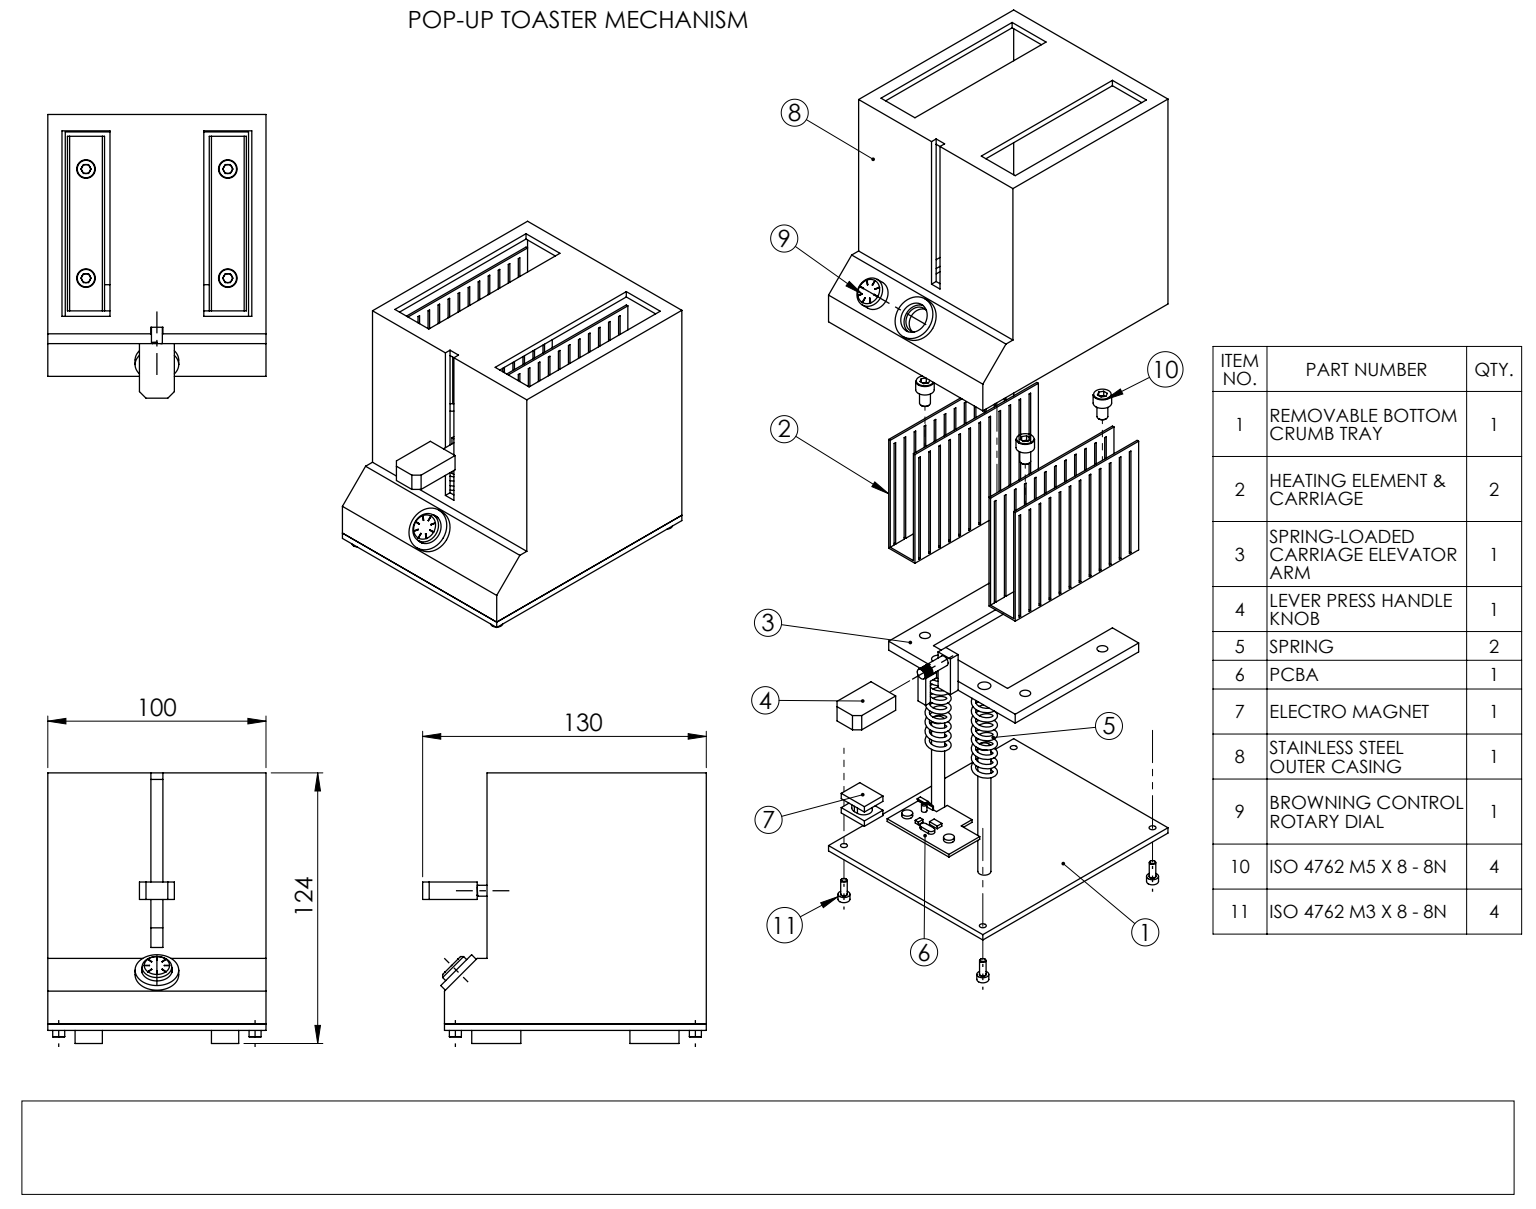
ISO-10303-21;
HEADER;
FILE_DESCRIPTION (('STEP AP214'),
    '1' );
FILE_NAME ('BR-818',
    '2026-10-08T14:41:38',
    ( '' ),
    ( '' ),
    'SwSTEP 2.0',
    'SolidWorks 2026',
    '' );
FILE_SCHEMA (( 'AUTOMOTIVE_DESIGN' ));
ENDSEC;

DATA;
#1 = CARTESIAN_POINT ( 'NONE',  ( -12.68318583509882380, -26.07549068051207541, 23.95507249208304756 ) ) ;
#2 = VECTOR ( 'NONE', #8948, 1000.000000000000000 ) ;
#3 = LINE ( 'NONE', #19320, #5933 ) ;
#4 = DIRECTION ( 'NONE',  ( -0.000000000000000000, 1.000000000000000000, -0.000000000000000000 ) ) ;
#5 = ORIENTED_EDGE ( 'NONE', *, *, #7068, .F. ) ;
#6 = CARTESIAN_POINT ( 'NONE',  ( -14.83517299489738761, -20.99999999999997513, 4.263677507916960430 ) ) ;
#7 = VECTOR ( 'NONE', #15495, 1000.000000000000000 ) ;
#8 = DIRECTION ( 'NONE',  ( 0.000000000000000000, 0.000000000000000000, -1.000000000000000000 ) ) ;
#9 = VERTEX_POINT ( 'NONE', #9196 ) ;
#10 = FACE_OUTER_BOUND ( 'NONE', #5278, .T. ) ;
#11 = VERTEX_POINT ( 'NONE', #7634 ) ;
#12 = LINE ( 'NONE', #3049, #2216 ) ;
#13 = DIRECTION ( 'NONE',  ( -1.000000000000000000, -2.168404344971008868E-16, 0.000000000000000000 ) ) ;
#14 = LINE ( 'NONE', #16487, #359 ) ;
#15 = PRODUCT_CONTEXT ( 'NONE', #3327, 'mechanical' ) ;
#16 = CARTESIAN_POINT ( 'NONE',  ( -25.00000000000000000, 53.00000000000000711, 30.00000000000000000 ) ) ;
#17 = EDGE_CURVE ( 'NONE', #5613, #1380, #13300, .T. ) ;
#18 = EDGE_CURVE ( 'NONE', #5079, #4517, #16249, .T. ) ;
#19 = AXIS2_PLACEMENT_3D ( 'NONE', #7359, #17758, #4328 ) ;
#21 = EDGE_CURVE ( 'NONE', #10175, #2143, #13600, .T. ) ;
#20 = CARTESIAN_POINT ( 'NONE',  ( -16.17491895705301275, -18.95583473709189803, 14.54492750791695421 ) ) ;
#22 = VECTOR ( 'NONE', #16690, 1000.000000000000000 ) ;
#23 = DIRECTION ( 'NONE',  ( -0.000000000000000000, -0.000000000000000000, -1.000000000000000000 ) ) ;
#24 = ORIENTED_EDGE ( 'NONE', *, *, #7353, .F. ) ;
#25 = CARTESIAN_POINT ( 'NONE',  ( -17.64274437364858983, -19.75228648362910633, 21.54882249208304401 ) ) ;
#26 = EDGE_CURVE ( 'NONE', #14106, #19091, #11969, .T. ) ;
#27 = MECHANICAL_DESIGN_GEOMETRIC_PRESENTATION_REPRESENTATION (  '', ( #18516 ), #10981 ) ;
#28 = CARTESIAN_POINT ( 'NONE',  ( -2.066987300000001415, 63.14382582708705627, 44.80000000109247082 ) ) ;
#29 = CARTESIAN_POINT ( 'NONE',  ( -17.35725562635140307, -28.41254052147349185, 40.79882249208304046 ) ) ;
#30 = CARTESIAN_POINT ( 'NONE',  ( 2.500000000000001776, 64.00000000000000000, 49.99999999999999289 ) ) ;
#31 = ORIENTED_EDGE ( 'NONE', *, *, #8748, .T. ) ;
#32 = VECTOR ( 'NONE', #13036, 1000.000000000000114 ) ;
#33 = DIRECTION ( 'NONE',  ( 0.000000000000000000, 0.4999999999999991118, -0.8660254037844391517 ) ) ;
#34 = ORIENTED_EDGE ( 'NONE', *, *, #9742, .F. ) ;
#35 = DIRECTION ( 'NONE',  ( -1.000000000000000000, 0.000000000000000000, -0.000000000000000000 ) ) ;
#36 = EDGE_CURVE ( 'NONE', #18345, #7828, #11830, .T. ) ;
#37 = DIRECTION ( 'NONE',  ( -1.000000000000000000, -0.000000000000000000, -0.000000000000000000 ) ) ;
#38 = AXIS2_PLACEMENT_3D ( 'NONE', #15476, #386, #16855 ) ;
#39 = CARTESIAN_POINT ( 'NONE',  ( -25.00000000000000000, 53.00000000000000711, -11.49999999999999645 ) ) ;
#40 = CARTESIAN_POINT ( 'NONE',  ( 2.500000000000000000, 0.000000000000000000, 0.000000000000000000 ) ) ;
#41 = CARTESIAN_POINT ( 'NONE',  ( 1.461580736456473684, 65.46158073645646880, 45.45000000109246940 ) ) ;
#42 = PRODUCT_DEFINITION_SHAPE ( 'NONE', 'NONE',  #19402 ) ;
#43 = CARTESIAN_POINT ( 'NONE',  ( 37.50000000000000711, -6.000000000000000000, -45.00000000000000000 ) ) ;
#44 = EDGE_CURVE ( 'NONE', #885, #4327, #14471, .T. ) ;
#45 = CARTESIAN_POINT ( 'NONE',  ( 4.592425496802577917E-16, 61.50000000000000000, 46.19999999999999574 ) ) ;
#46 = PLANE ( 'NONE',  #8954 ) ;
#47 = AXIS2_PLACEMENT_3D ( 'NONE', #8306, #16043, #2603 ) ;
#48 = B_SPLINE_CURVE_WITH_KNOTS ( 'NONE', 3,
 ( #13537, #4634, #4733, #16687 ),
 .UNSPECIFIED., .F., .F.,
 ( 4, 4 ),
 ( 0.000000000000000000, 1.000000000000000000 ),
 .UNSPECIFIED. ) ;
#49 = EDGE_LOOP ( 'NONE', ( #2329, #11638, #12440, #4824 ) ) ;
#50 = AXIS2_PLACEMENT_3D ( 'NONE', #5480, #14305, #2436 ) ;
#51 = DIRECTION ( 'NONE',  ( 6.123233995736766036E-17, 1.000000000000000000, 0.000000000000000000 ) ) ;
#52 = CARTESIAN_POINT ( 'NONE',  ( -10.75228648362910100, -26.64274437364854009, 6.013677507916958653 ) ) ;
#53 = CARTESIAN_POINT ( 'NONE',  ( -19.41254052147348830, -26.35725562635142083, 18.26367750791695599 ) ) ;
#54 = CARTESIAN_POINT ( 'NONE',  ( 1.767766952966369987, 65.76776695296638309, 49.00000000218494023 ) ) ;
#55 = CARTESIAN_POINT ( 'NONE',  ( -13.49542703274174116, -28.95583473709188738, 3.392572492083040903 ) ) ;
#56 = ADVANCED_FACE ( 'NONE', ( #13399 ), #17297, .T. ) ;
#57 = EDGE_CURVE ( 'NONE', #1624, #17649, #87, .T. ) ;
#58 = CARTESIAN_POINT ( 'NONE',  ( 2.066987300000002303, 63.14382582708705627, 45.30000000109247082 ) ) ;
#59 = CARTESIAN_POINT ( 'NONE',  ( -13.82508104294698192, -29.04416526290806644, 1.419927507916958209 ) ) ;
#60 = CARTESIAN_POINT ( 'NONE',  ( -41.00000000000000711, 110.0000000000000000, 6.999999999999999112 ) ) ;
#61 = CARTESIAN_POINT ( 'NONE',  ( -15.16482700510259640, -28.99999999999998224, 1.638677507916958431 ) ) ;
#62 = CARTESIAN_POINT ( 'NONE',  ( -37.50000000000002132, 0.000000000000000000, 44.99999999999997868 ) ) ;
#63 = VECTOR ( 'NONE', #9225, 1000.000000000000114 ) ;
#64 = EDGE_CURVE ( 'NONE', #9274, #14710, #15088, .T. ) ;
#65 = DIRECTION ( 'NONE',  ( 1.000000000000000000, 0.000000000000000000, 0.000000000000000000 ) ) ;
#66 = CYLINDRICAL_SURFACE ( 'NONE', #13079, 2.500000000000000444 ) ;
#67 = AXIS2_PLACEMENT_3D ( 'NONE', #5864, #11526, #16244 ) ;
#68 = FACE_OUTER_BOUND ( 'NONE', #2154, .T. ) ;
#69 = CARTESIAN_POINT ( 'NONE',  ( 2.066987300000001859, 63.14382582708704916, 46.10000000109246798 ) ) ;
#70 = LINE ( 'NONE', #3095, #14117 ) ;
#71 = DIRECTION ( 'NONE',  ( -1.000000000000000000, -0.000000000000000000, -0.000000000000000000 ) ) ;
#72 = VERTEX_POINT ( 'NONE', #4700 ) ;
#73 = ORIENTED_EDGE ( 'NONE', *, *, #1505, .T. ) ;
#74 = CARTESIAN_POINT ( 'NONE',  ( -7.999999999999996447, -23.83517299489733432, 23.29882249208304046 ) ) ;
#75 = FACE_OUTER_BOUND ( 'NONE', #12049, .T. ) ;
#77 = ORIENTED_EDGE ( 'NONE', *, *, #16848, .F. ) ;
#76 = VERTEX_POINT ( 'NONE', #16452 ) ;
#78 = ADVANCED_FACE ( 'NONE', ( #3019 ), #8997, .T. ) ;
#79 = CARTESIAN_POINT ( 'NONE',  ( -15.63902057219076269, -20.95583473709189448, 9.294927507916961318 ) ) ;
#80 = FACE_OUTER_BOUND ( 'NONE', #9007, .T. ) ;
#81 = CARTESIAN_POINT ( 'NONE',  ( -21.14459132904239169, -20.64274437364858628, 5.361322492083039570 ) ) ;
#82 = CARTESIAN_POINT ( 'NONE',  ( 2.500000000000006661, 65.03553390593272354, 48.04999999999999716 ) ) ;
#83 = CARTESIAN_POINT ( 'NONE',  ( 2.066987300000001859, 64.85617417291294373, 46.80000000109246372 ) ) ;
#84 = ORIENTED_EDGE ( 'NONE', *, *, #1267, .T. ) ;
#85 = EDGE_LOOP ( 'NONE', ( #12730, #3911, #462, #6972, #16450, #10959, #3705, #8319, #7529, #13845, #6781, #19380, #3029, #10375 ) ) ;
#86 = LINE ( 'NONE', #12030, #9433 ) ;
#87 = LINE ( 'NONE', #2922, #12898 ) ;
#88 = CLOSED_SHELL ( 'NONE', ( #433, #16433, #12643, #3854, #16960, #8083, #12476, #2887, #13363, #11571, #11070, #10821, #5435, #14081, #18479, #16340, #3288, #10464, #13954, #1717, #18414, #1458, #6350, #11815, #16187, #14084, #2136, #6137, #1464, #12159, #2663, #1129, #18269, #562, #5420, #78, #10177, #12810, #725, #8545, #7974, #4556, #12238, #18488, #11655, #2010 ) ) ;
#89 = VERTEX_POINT ( 'NONE', #13508 ) ;
#90 = CARTESIAN_POINT ( 'NONE',  ( -15.00000000000001066, -19.99999999999997868, -4.814824860968089633E-32 ) ) ;
#91 = DIRECTION ( 'NONE',  ( 0.000000000000000000, -0.4999999999999993894, 0.8660254037844389297 ) ) ;
#92 = CARTESIAN_POINT ( 'NONE',  ( -2.066987300000001415, 63.14382582708705627, 46.60000000109246088 ) ) ;
#93 = CARTESIAN_POINT ( 'NONE',  ( 4.072081901468762588, 26.82127119883315558, 59.66337542264481186 ) ) ;
#94 = FACE_OUTER_BOUND ( 'NONE', #15883, .T. ) ;
#95 = ORIENTED_EDGE ( 'NONE', *, *, #5527, .F. ) ;
#97 = ORIENTED_EDGE ( 'NONE', *, *, #1658, .T. ) ;
#96 = EDGE_LOOP ( 'NONE', ( #12565, #3709, #10938 ) ) ;
#98 = CARTESIAN_POINT ( 'NONE',  ( -9.754982604823348780, -18.99630608921234654, 15.41992750791695777 ) ) ;
#99 = CARTESIAN_POINT ( 'NONE',  ( 44.99999999999997158, 6.000000000000000000, 55.00000000000000000 ) ) ;
#100 = EDGE_LOOP ( 'NONE', ( #14836, #13611, #8992, #9930 ) ) ;
#101 = ORIENTED_EDGE ( 'NONE', *, *, #16409, .T. ) ;
#102 = ADVANCED_FACE ( 'NONE', ( #6068 ), #4601, .T. ) ;
#103 = CARTESIAN_POINT ( 'NONE',  ( -14.83517299489736985, -26.99999999999998579, 24.61132249208304756 ) ) ;
#104 = CARTESIAN_POINT ( 'NONE',  ( -1.767766952966370209, 65.76776695296638309, 45.09999999999999432 ) ) ;
#105 = CARTESIAN_POINT ( 'NONE',  ( 2.500000000000002220, 62.96446609406726225, 47.25000000218494023 ) ) ;
#106 = VERTEX_POINT ( 'NONE', #9669 ) ;
#107 = CARTESIAN_POINT ( 'NONE',  ( -11.99999999999999289, -24.16482700510258752, 16.07617750791696309 ) ) ;
#108 = CARTESIAN_POINT ( 'NONE',  ( 1.035533905932738197, 66.50000000000000000, 47.45000000218494307 ) ) ;
#109 = VERTEX_POINT ( 'NONE', #11046 ) ;
#110 = CYLINDRICAL_SURFACE ( 'NONE', #17224, 7.000000000000001776 ) ;
#111 = VERTEX_POINT ( 'NONE', #2135 ) ;
#112 = DIRECTION ( 'NONE',  ( 0.000000000000000000, -0.000000000000000000, 1.000000000000000000 ) ) ;
#113 = DIRECTION ( 'NONE',  ( -0.000000000000000000, -0.000000000000000000, -1.000000000000000000 ) ) ;
#114 = CARTESIAN_POINT ( 'NONE',  ( -24.00000000000000000, 53.00000000000000711, -18.00000000000000355 ) ) ;
#115 = DIRECTION ( 'NONE',  ( 0.000000000000000000, 0.000000000000000000, -1.000000000000000000 ) ) ;
#116 = CARTESIAN_POINT ( 'NONE',  ( -44.99999999999998579, 0.000000000000000000, -55.00000000000000000 ) ) ;
#117 =( BOUNDED_SURFACE ( )  B_SPLINE_SURFACE ( 1, 2, ( 
 ( #9163, #1629, #4271, #7495, #8867, #13566, #54, #147, #16622, #6038, #10621, #5837, #11801, #11995, #17795, #6132, #7697, #11700, #4368, #8766, #10328, #18092, #13663, #17993, #16519, #4567, #7300, #3082, #9063, #3189, #15146, #1716, #14852, #17693, #14756, #16325, #2892, #12485, #3479, #12194, #442, #7902, #14057, #8092, #12393, #13866, #14158, #7997, #9347, #18390, #537, #2108, #16718, #6621, #631, #6520, #347, #6427, #4959, #12590, #4862, #4774, #15339, #1815, #3572, #3380, #18195, #18582, #10724, #1916, #2196, #10915, #5055, #16914, #7795, #9453, #10818, #16816, #5148, #11110, #11015, #17106, #3286, #13963, #15243, #15441, #9257, #13766, #15626, #18487, #2006, #6333, #12299, #15537, #18294, #17014, #3670, #9545, #9641, #8190, #6229 ),
 ( #18952, #2384, #1012, #18680, #11198, #18866, #15731, #11580, #14338, #911, #11481, #3953, #5519, #3859, #728, #2668, #5428, #9821, #6987, #17378, #6707, #6893, #8369, #8555, #2573, #12865, #11386, #8648, #2474, #15818, #9915, #14438, #16015, #17201, #1102, #14530, #12953, #14247, #15910, #8462, #7083, #18763, #5245, #17469, #2291, #4045, #17293, #12678, #13046, #3766, #10011, #16101, #19045, #5618, #17578, #8277, #4155, #5336, #11297, #10105, #9735, #818, #6803, #12767, #2961, #4248, #7378, #13151, #17669, #4646, #7471, #2867, #14730, #10206, #4543, #16197, #1401, #10502, #1308, #8739, #4344, #15028, #11876, #7281, #16500, #9040, #13444, #16295, #14933, #19149, #5720, #13349, #2764, #6109, #13247, #28, #19343, #10403, #19244, #1504, #12075 ) ),
 .UNSPECIFIED., .F., .F., .F. ) 
 B_SPLINE_SURFACE_WITH_KNOTS ( ( 2, 2 ),
 ( 3, 2, 2, 2, 2, 2, 2, 2, 2, 2, 2, 2, 2, 2, 2, 2, 2, 2, 2, 2, 2, 2, 2, 2, 2, 2, 2, 2, 2, 2, 2, 2, 2, 2, 2, 2, 2, 2, 2, 2, 2, 2, 2, 2, 2, 2, 2, 2, 2, 2, 3 ),
 ( 0.000000000000000000, 1.000000000000000000 ),
 ( 0.000000000000000000, 0.01785714285714285615, 0.03571428571428571230, 0.05357142857142856845, 0.07142857142857142461, 0.08928571428571428770, 0.1071428571428571369, 0.1250000000000000000, 0.1428571428571428492, 0.1607142857142857262, 0.1785714285714285754, 0.1964285714285714246, 0.2142857142857142738, 0.2321428571428571508, 0.2500000000000000000, 0.2678571428571428492, 0.2857142857142856984, 0.3035714285714285476, 0.3214285714285714524, 0.3392857142857143016, 0.3571428571428571508, 0.3750000000000000000, 0.3928571428571428492, 0.4107142857142856984, 0.4285714285714285476, 0.4464285714285714524, 0.4642857142857143016, 0.4821428571428571508, 0.5000000000000000000, 0.5178571428571429047, 0.5357142857142856984, 0.5535714285714286031, 0.5714285714285713969, 0.5892857142857143016, 0.6071428571428570953, 0.6250000000000000000, 0.6428571428571429047, 0.6607142857142856984, 0.6785714285714286031, 0.6964285714285713969, 0.7142857142857143016, 0.7321428571428570953, 0.7500000000000000000, 0.7678571428571429047, 0.7857142857142856984, 0.8035714285714286031, 0.8214285714285713969, 0.8392857142857143016, 0.8571428571428570953, 0.8750000000000000000, 0.8928571428571429047 ),
 .UNSPECIFIED. ) 
 GEOMETRIC_REPRESENTATION_ITEM ( )  RATIONAL_B_SPLINE_SURFACE ( (
 ( 1.000000000000000000, 0.9238795325112867385, 1.000000000000000000, 0.9238795325112867385, 1.000000000000000000, 0.9238795325112867385, 1.000000000000000000, 0.9238795325112867385, 1.000000000000000000, 0.9238795325112867385, 1.000000000000000000, 0.9238795325112867385, 1.000000000000000000, 0.9238795325112867385, 1.000000000000000000, 0.9238795325112867385, 1.000000000000000000, 0.9238795325112867385, 1.000000000000000000, 0.9238795325112867385, 1.000000000000000000, 0.9238795325112867385, 1.000000000000000000, 0.9238795325112867385, 1.000000000000000000, 0.9238795325112867385, 1.000000000000000000, 0.9238795325112867385, 1.000000000000000000, 0.9238795325112867385, 1.000000000000000000, 0.9238795325112867385, 1.000000000000000000, 0.9238795325112867385, 1.000000000000000000, 0.9238795325112867385, 1.000000000000000000, 0.9238795325112867385, 1.000000000000000000, 0.9238795325112867385, 1.000000000000000000, 0.9238795325112867385, 1.000000000000000000, 0.9238795325112867385, 1.000000000000000000, 0.9238795325112867385, 1.000000000000000000, 0.9238795325112867385, 1.000000000000000000, 0.9238795325112867385, 1.000000000000000000, 0.9238795325112867385, 1.000000000000000000, 0.9238795325112867385, 1.000000000000000000, 0.9238795325112867385, 1.000000000000000000, 0.9238795325112867385, 1.000000000000000000, 0.9238795325112867385, 1.000000000000000000, 0.9238795325112867385, 1.000000000000000000, 0.9238795325112867385, 1.000000000000000000, 0.9238795325112867385, 1.000000000000000000, 0.9238795325112867385, 1.000000000000000000, 0.9238795325112867385, 1.000000000000000000, 0.9238795325112867385, 1.000000000000000000, 0.9238795325112867385, 1.000000000000000000, 0.9238795325112867385, 1.000000000000000000, 0.9238795325112867385, 1.000000000000000000, 0.9238795325112867385, 1.000000000000000000, 0.9238795325112867385, 1.000000000000000000, 0.9238795325112867385, 1.000000000000000000, 0.9238795325112867385, 1.000000000000000000, 0.9238795325112867385, 1.000000000000000000, 0.9238795325112867385, 1.000000000000000000, 0.9238795325112867385, 1.000000000000000000, 0.9238795325112867385, 1.000000000000000000, 0.9238795325112867385, 1.000000000000000000, 0.9238795325112867385, 1.000000000000000000, 0.9238795325112867385, 1.000000000000000000),
 ( 1.000000000000000000, 0.9238795325112867385, 1.000000000000000000, 0.9238795325112867385, 1.000000000000000000, 0.9238795325112867385, 1.000000000000000000, 0.9238795325112867385, 1.000000000000000000, 0.9238795325112867385, 1.000000000000000000, 0.9238795325112867385, 1.000000000000000000, 0.9238795325112867385, 1.000000000000000000, 0.9238795325112867385, 1.000000000000000000, 0.9238795325112867385, 1.000000000000000000, 0.9238795325112867385, 1.000000000000000000, 0.9238795325112867385, 1.000000000000000000, 0.9238795325112867385, 1.000000000000000000, 0.9238795325112867385, 1.000000000000000000, 0.9238795325112867385, 1.000000000000000000, 0.9238795325112867385, 1.000000000000000000, 0.9238795325112867385, 1.000000000000000000, 0.9238795325112867385, 1.000000000000000000, 0.9238795325112867385, 1.000000000000000000, 0.9238795325112867385, 1.000000000000000000, 0.9238795325112867385, 1.000000000000000000, 0.9238795325112867385, 1.000000000000000000, 0.9238795325112867385, 1.000000000000000000, 0.9238795325112867385, 1.000000000000000000, 0.9238795325112867385, 1.000000000000000000, 0.9238795325112867385, 1.000000000000000000, 0.9238795325112867385, 1.000000000000000000, 0.9238795325112867385, 1.000000000000000000, 0.9238795325112867385, 1.000000000000000000, 0.9238795325112867385, 1.000000000000000000, 0.9238795325112867385, 1.000000000000000000, 0.9238795325112867385, 1.000000000000000000, 0.9238795325112867385, 1.000000000000000000, 0.9238795325112867385, 1.000000000000000000, 0.9238795325112867385, 1.000000000000000000, 0.9238795325112867385, 1.000000000000000000, 0.9238795325112867385, 1.000000000000000000, 0.9238795325112867385, 1.000000000000000000, 0.9238795325112867385, 1.000000000000000000, 0.9238795325112867385, 1.000000000000000000, 0.9238795325112867385, 1.000000000000000000, 0.9238795325112867385, 1.000000000000000000, 0.9238795325112867385, 1.000000000000000000, 0.9238795325112867385, 1.000000000000000000, 0.9238795325112867385, 1.000000000000000000, 0.9238795325112867385, 1.000000000000000000, 0.9238795325112867385, 1.000000000000000000, 0.9238795325112867385, 1.000000000000000000, 0.9238795325112867385, 1.000000000000000000, 0.9238795325112867385, 1.000000000000000000, 0.9238795325112867385, 1.000000000000000000) ) ) 
 REPRESENTATION_ITEM ( '' )  SURFACE ( )  );
#118 = DIRECTION ( 'NONE',  ( -1.000000000000000000, -0.000000000000000000, -0.000000000000000000 ) ) ;
#119 = PLANE ( 'NONE',  #7046 ) ;
#120 = CARTESIAN_POINT ( 'NONE',  ( -19.95583473709191580, -22.49542703274176603, 13.66992750791695599 ) ) ;
#121 = DIRECTION ( 'NONE',  ( -0.000000000000000000, -1.000000000000000000, -0.000000000000000000 ) ) ;
#122 = ORIENTED_EDGE ( 'NONE', *, *, #7448, .F. ) ;
#123 = CARTESIAN_POINT ( 'NONE',  ( -16.50457296725825174, -19.04416526290807354, 16.51757249208304046 ) ) ;
#124 = EDGE_CURVE ( 'NONE', #10346, #18340, #3322, .T. ) ;
#125 = CARTESIAN_POINT ( 'NONE',  ( 4.101219330881969327, 32.64264068711926825, 53.84264068711931372 ) ) ;
#126 = CARTESIAN_POINT ( 'NONE',  ( -14.83517299489736985, -26.99999999999998579, 19.36132249208304046 ) ) ;
#127 = DIRECTION ( 'NONE',  ( -0.000000000000000000, -0.000000000000000000, -1.000000000000000000 ) ) ;
#128 = ORIENTED_EDGE ( 'NONE', *, *, #13504, .F. ) ;
#129 = CARTESIAN_POINT ( 'NONE',  ( -11.21456601361727046, -19.57682413056721416, 1.010946030696228434E-16 ) ) ;
#130 = ORIENTED_EDGE ( 'NONE', *, *, #2687, .F. ) ;
#131 = DIRECTION ( 'NONE',  ( -0.000000000000000000, -0.000000000000000000, -1.000000000000000000 ) ) ;
#132 = EDGE_CURVE ( 'NONE', #16262, #13646, #5091, .T. ) ;
#133 = CARTESIAN_POINT ( 'NONE',  ( -45.00000000000000000, 6.000000000000000000, 54.99999999999998579 ) ) ;
#134 = DIRECTION ( 'NONE',  ( 0.000000000000000000, -1.000000000000000000, 0.000000000000000000 ) ) ;
#135 = CARTESIAN_POINT ( 'NONE',  ( 0.000000000000000000, 64.00000000000000000, 49.99999999999999289 ) ) ;
#136 = AXIS2_PLACEMENT_3D ( 'NONE', #17568, #5609, #6979 ) ;
#137 = CARTESIAN_POINT ( 'NONE',  ( -2.066987300000001415, 64.85617417291294373, 48.10000000109246798 ) ) ;
#138 = EDGE_CURVE ( 'NONE', #19239, #1798, #9382, .T. ) ;
#139 = CARTESIAN_POINT ( 'NONE',  ( -2.500000000000001776, 64.00000000000000000, 46.79999999999999716 ) ) ;
#140 = CARTESIAN_POINT ( 'NONE',  ( 4.592425496802577917E-16, 61.50000000000000000, 46.99999999999999289 ) ) ;
#141 = DIRECTION ( 'NONE',  ( 0.000000000000000000, -1.000000000000000000, -0.000000000000000000 ) ) ;
#142 = ORIENTED_EDGE ( 'NONE', *, *, #12510, .F. ) ;
#143 = DIRECTION ( 'NONE',  ( 0.000000000000000000, 0.000000000000000000, 1.000000000000000000 ) ) ;
#144 = CARTESIAN_POINT ( 'NONE',  ( -17.35725562635144215, -19.58745947852648683, 19.57617750791695954 ) ) ;
#145 = VECTOR ( 'NONE', #11392, 1000.000000000000000 ) ;
#146 = CARTESIAN_POINT ( 'NONE',  ( -17.35725562635144215, -19.58745947852648683, 9.076177507916957765 ) ) ;
#147 = CARTESIAN_POINT ( 'NONE',  ( 2.500000000000001776, 65.03553390593273775, 48.95000000218495018 ) ) ;
#148 = EDGE_CURVE ( 'NONE', #1741, #16697, #12522, .T. ) ;
#149 = CARTESIAN_POINT ( 'NONE',  ( -20.24501739517669563, -18.99630608921239627, 42.33007249208303335 ) ) ;
#150 = DIRECTION ( 'NONE',  ( 0.000000000000000000, 0.000000000000000000, 1.000000000000000000 ) ) ;
#151 = CARTESIAN_POINT ( 'NONE',  ( -10.58745947852649927, -21.64274437364853654, -0.1113224920830418047 ) ) ;
#152 = CYLINDRICAL_SURFACE ( 'NONE', #8291, 1.500000000000001332 ) ;
#153 = CARTESIAN_POINT ( 'NONE',  ( -12.35725562635143682, -19.75228648362908501, 20.45117750791695954 ) ) ;
#154 = PLANE ( 'NONE',  #4763 ) ;
#155 = FACE_BOUND ( 'NONE', #7820, .T. ) ;
#156 = CARTESIAN_POINT ( 'NONE',  ( -2.066987300000001859, 64.85617417291294373, 48.90000000109247225 ) ) ;
#157 = DIRECTION ( 'NONE',  ( 1.000000000000000000, 0.000000000000000000, -7.709882115452476934E-17 ) ) ;
#158 = AXIS2_PLACEMENT_3D ( 'NONE', #9160, #1711, #12091 ) ;
#159 = PLANE ( 'NONE',  #4117 ) ;
#160 = VECTOR ( 'NONE', #17759, 1000.000000000000000 ) ;
#161 = CARTESIAN_POINT ( 'NONE',  ( 1.461580736456473906, 62.53841926354353120, 45.25000000109247367 ) ) ;
#162 = CARTESIAN_POINT ( 'NONE',  ( -1.461580736456473906, 65.46158073645646880, 49.65000000109246514 ) ) ;
#163 = LINE ( 'NONE', #1934, #7064 ) ;
#164 = EDGE_CURVE ( 'NONE', #17715, #9777, #4992, .T. ) ;
#165 = EDGE_CURVE ( 'NONE', #16279, #13992, #8531, .T. ) ;
#166 = DIRECTION ( 'NONE',  ( 0.000000000000000000, -0.7071067811865495711, 0.7071067811865454633 ) ) ;
#167 = EDGE_LOOP ( 'NONE', ( #6125, #3258, #15700, #3937 ) ) ;
#168 = ORIENTED_EDGE ( 'NONE', *, *, #9841, .T. ) ;
#169 = ADVANCED_FACE ( 'NONE', ( #13798 ), #17134, .T. ) ;
#170 = CARTESIAN_POINT ( 'NONE',  ( -22.04416526290809486, -22.28918265808477628, 15.64257249208304223 ) ) ;
#171 =( NAMED_UNIT ( * ) SI_UNIT ( $, .STERADIAN. ) SOLID_ANGLE_UNIT ( ) );
#172 = DIRECTION ( 'NONE',  ( -2.973811673103096679E-16, 0.000000000000000000, 1.000000000000000000 ) ) ;
#174 = EDGE_LOOP ( 'NONE', ( #3560, #14789, #10322, #7746, #12837, #13051 ) ) ;
#173 = ORIENTED_EDGE ( 'NONE', *, *, #18111, .T. ) ;
#175 = CARTESIAN_POINT ( 'NONE',  ( -18.04416526290808420, -24.63902057219074493, 18.48242750791695954 ) ) ;
#176 = CARTESIAN_POINT ( 'NONE',  ( -41.00000000000000711, 53.00000000000000711, 8.000000000000000000 ) ) ;
#177 = CARTESIAN_POINT ( 'NONE',  ( -7.999999999999996447, -23.83517299489733432, 7.548822492083037794 ) ) ;
#178 = AXIS2_PLACEMENT_3D ( 'NONE', #10166, #16166, #2735 ) ;
#179 = DIRECTION ( 'NONE',  ( -0.000000000000000000, -0.000000000000000000, -1.000000000000000000 ) ) ;
#180 = CARTESIAN_POINT ( 'NONE',  ( -2.066987300000001415, 64.00000000000000000, 46.35000000109246798 ) ) ;
#181 = ORIENTED_EDGE ( 'NONE', *, *, #18284, .T. ) ;
#182 = ORIENTED_EDGE ( 'NONE', *, *, #1003, .F. ) ;
#183 = DIRECTION ( 'NONE',  ( 0.000000000000000000, 1.000000000000000000, 1.632680918566406793E-16 ) ) ;
#184 = VERTEX_POINT ( 'NONE', #3603 ) ;
#185 = VERTEX_POINT ( 'NONE', #9574 ) ;
#186 = CARTESIAN_POINT ( 'NONE',  ( 0.000000000000000000, 47.00000000000000711, -50.00000000000000000 ) ) ;
#187 = LINE ( 'NONE', #12134, #5316 ) ;
#188 = CARTESIAN_POINT ( 'NONE',  ( 2.066987300000001859, 64.85617417291294373, 46.20000000109247651 ) ) ;
#189 = EDGE_CURVE ( 'NONE', #14847, #7431, #12616, .T. ) ;
#190 = ADVANCED_FACE ( 'NONE', ( #565 ), #6556, .T. ) ;
#191 = CARTESIAN_POINT ( 'NONE',  ( 4.012354697599916697, 26.78000129688588871, 59.70432772728319293 ) ) ;
#192 = AXIS2_PLACEMENT_3D ( 'NONE', #9179, #627, #10638 ) ;
#193 = VECTOR ( 'NONE', #5352, 1000.000000000000000 ) ;
#194 = FACE_OUTER_BOUND ( 'NONE', #3643, .T. ) ;
#195 = ORIENTED_EDGE ( 'NONE', *, *, #2336, .T. ) ;
#197 = EDGE_LOOP ( 'NONE', ( #16436, #17465, #12376, #16579 ) ) ;
#196 = EDGE_LOOP ( 'NONE', ( #2060, #11072, #774, #8129 ) ) ;
#198 = CARTESIAN_POINT ( 'NONE',  ( -20.97976432393977575, -20.35725562635143504, 13.88867750791695599 ) ) ;
#199 = DIRECTION ( 'NONE',  ( 0.000000000000000000, 1.000000000000000000, -0.000000000000000000 ) ) ;
#200 = ORIENTED_EDGE ( 'NONE', *, *, #5789, .F. ) ;
#201 = VERTEX_POINT ( 'NONE', #6735 ) ;
#202 = CARTESIAN_POINT ( 'NONE',  ( -13.64274437364857739, -21.31951028609534760, 11.92382249208304401 ) ) ;
#203 = CARTESIAN_POINT ( 'NONE',  ( 0.8561741729129471734, 61.93301270000000613, 49.00000000109246656 ) ) ;
#204 = DIRECTION ( 'NONE',  ( 0.000000000000000000, 0.000000000000000000, 1.000000000000000000 ) ) ;
#205 = ORIENTED_EDGE ( 'NONE', *, *, #8210, .F. ) ;
#206 = CARTESIAN_POINT ( 'NONE',  ( -15.96867458239597326, -26.95583473709190159, 17.60742750791696309 ) ) ;
#207 = CIRCLE ( 'NONE', #14282, 4.000000000000001776 ) ;
#208 = CARTESIAN_POINT ( 'NONE',  ( -2.500000000000001776, 64.00000000000000000, 44.50000000218494733 ) ) ;
#209 = VERTEX_POINT ( 'NONE', #3697 ) ;
#210 = CIRCLE ( 'NONE', #18070, 1.678500596222258556 ) ;
#211 = LINE ( 'NONE', #15300, #5330 ) ;
#212 = ORIENTED_EDGE ( 'NONE', *, *, #12916, .T. ) ;
#213 = CARTESIAN_POINT ( 'NONE',  ( -2.500000000000001776, 64.00000000000000000, 46.79999999999999716 ) ) ;
#214 = PLANE ( 'NONE',  #4233 ) ;
#215 = CARTESIAN_POINT ( 'NONE',  ( -10.00000000000000000, 50.00000000000000000, 30.00000000000000000 ) ) ;
#216 = ITEM_DEFINED_TRANSFORMATION ( 'NONE', 'NONE', #18938,  #1791 ) ;
#217 = EDGE_CURVE ( 'NONE', #3132, #14286, #15567, .T. ) ;
#218 = CARTESIAN_POINT ( 'NONE',  ( -40.00000000000000000, 53.00000000000000711, 20.00000000000000000 ) ) ;
#219 = DIRECTION ( 'NONE',  ( -1.000000000000000000, -0.000000000000000000, -0.000000000000000000 ) ) ;
#220 = CARTESIAN_POINT ( 'NONE',  ( -2.500000000000019096, 65.03553390593272354, 48.35000000000000853 ) ) ;
#221 = LINE ( 'NONE', #319, #18355 ) ;
#222 = CARTESIAN_POINT ( 'NONE',  ( -10.04416526290807710, -25.50457296725819489, 21.54492750791695599 ) ) ;
#223 = LINE ( 'NONE', #13638, #15855 ) ;
#224 = ORIENTED_EDGE ( 'NONE', *, *, #676, .F. ) ;
#225 = AXIS2_PLACEMENT_3D ( 'NONE', #6440, #18405, #16930 ) ;
#226 = CARTESIAN_POINT ( 'NONE',  ( -19.95583473709190514, -25.50457296725822687, 15.20507249208304046 ) ) ;
#227 = DIRECTION ( 'NONE',  ( 0.000000000000000000, 0.000000000000000000, -1.000000000000000000 ) ) ;
#228 = CARTESIAN_POINT ( 'NONE',  ( -17.07549068051208963, -26.31681416490115311, 25.26757249208305112 ) ) ;
#229 = CARTESIAN_POINT ( 'NONE',  ( 1.767766952966369987, 65.76776695296638309, 45.69999999999999574 ) ) ;
#230 = EDGE_LOOP ( 'NONE', ( #8619, #14141, #10740, #17845 ) ) ;
#231 = PLANE ( 'NONE',  #3745 ) ;
#232 = VERTEX_POINT ( 'NONE', #15660 ) ;
#233 = LINE ( 'NONE', #4758, #9368 ) ;
#234 = CARTESIAN_POINT ( 'NONE',  ( -40.00000000000000000, 53.00000000000000711, -32.00000000000000000 ) ) ;
#235 =( BOUNDED_CURVE ( )  B_SPLINE_CURVE ( 2, ( #4277, #17906, #10238, #11607, #11805, #16129, #13075, #8674, #61, #14656, #4180, #7208, #16424, #14762, #1334, #10042, #1227, #16223, #2599, #7501, #2989, #1531, #2897, #2794, #14856, #14957, #8970, #6044, #13479, #16039, #8872, #13181, #1431, #8580, #19173, #17497, #1133, #19368, #4075, #5744, #11704, #5939, #14561, #7112, #8771, #7304, #13271, #5844, #17801, #4375, #10334, #11910, #16330, #7406, #18202, #8002, #16628, #18399, #15345, #16823, #3194, #18000, #9264, #6339, #12200, #9460, #9170, #1636, #352, #13969, #13671, #4779, #250, #10531, #6235, #18299, #7607, #12304, #1822, #4965, #10729, #542, #12001, #16524, #4867, #7801, #13772, #4574, #15251, #3386, #10827, #16725, #6140, #9355, #153, #1924, #7907, #15154, #3087, #9070, #13872, #10922, #3294, #16922, #447, #1723, #6432, #3485, #12399, #7704, #15446, #2013, #15057, #13572, #12101, #18097, #4670, #10626, #2113, #12596, #918, #14165, #17022, #6900, #17387, #6629, #11203, #15918, #2390, #3579, #9551, #5251, #14345, #2299, #5064, #17112, #8376, #3772, #12683, #18872, #12873, #18494, #17302, #3676, #3864, #15543, #8198, #8469, #8097, #5437, #3961, #18587, #14066, #8283, #9921, #14253, #638, #825, #11393, #17207, #9830, #2481, #734, #14445, #6528, #15823, #18686, #12493, #11115, #11020, #5154, #11304, #9646, #15633, #2205, #6808, #6713, #9745, #15737, #5341, #12773, #18769, #2674, #1205, #8657, #18960, #14638, #7289, #16022 ),
 .UNSPECIFIED., .F., .F. ) 
 B_SPLINE_CURVE_WITH_KNOTS ( ( 3, 2, 2, 2, 2, 2, 2, 2, 2, 2, 2, 2, 2, 2, 2, 2, 2, 2, 2, 2, 2, 2, 2, 2, 2, 2, 2, 2, 2, 2, 2, 2, 2, 2, 2, 2, 2, 2, 2, 2, 2, 2, 2, 2, 2, 2, 2, 2, 2, 2, 2, 2, 2, 2, 2, 2, 2, 2, 2, 2, 2, 2, 2, 2, 2, 2, 2, 2, 2, 2, 2, 2, 2, 2, 2, 2, 2, 2, 2, 2, 2, 2, 2, 2, 2, 2, 2, 2, 2, 2, 2, 2, 2, 2, 3 ),
 ( 0.02351720863160803449, 0.03125000000000000000, 0.04166666666666666435, 0.05208333333333333565, 0.06250000000000000000, 0.07291666666666665741, 0.08333333333333332871, 0.09375000000000000000, 0.1041666666666666574, 0.1145833333333333148, 0.1250000000000000000, 0.1354166666666666574, 0.1458333333333333426, 0.1562500000000000000, 0.1666666666666666574, 0.1770833333333333426, 0.1875000000000000000, 0.1979166666666666574, 0.2083333333333333426, 0.2187500000000000000, 0.2291666666666666574, 0.2395833333333333426, 0.2500000000000000000, 0.2604166666666666852, 0.2708333333333333148, 0.2812500000000000000, 0.2916666666666666852, 0.3020833333333333148, 0.3125000000000000000, 0.3229166666666666852, 0.3333333333333333148, 0.3437500000000000000, 0.3541666666666666852, 0.3645833333333333148, 0.3750000000000000000, 0.3854166666666666852, 0.3958333333333333148, 0.4062500000000000000, 0.4166666666666666852, 0.4270833333333333148, 0.4375000000000000000, 0.4479166666666666852, 0.4583333333333333148, 0.4687500000000000000, 0.4791666666666666852, 0.4895833333333333148, 0.5000000000000000000, 0.5104166666666666297, 0.5208333333333333703, 0.5312500000000000000, 0.5416666666666666297, 0.5520833333333333703, 0.5625000000000000000, 0.5729166666666666297, 0.5833333333333333703, 0.5937500000000000000, 0.6041666666666666297, 0.6145833333333333703, 0.6250000000000000000, 0.6354166666666666297, 0.6458333333333333703, 0.6562500000000000000, 0.6666666666666666297, 0.6770833333333333703, 0.6875000000000000000, 0.6979166666666666297, 0.7083333333333333703, 0.7187500000000000000, 0.7291666666666666297, 0.7395833333333333703, 0.7500000000000000000, 0.7604166666666666297, 0.7708333333333333703, 0.7812500000000000000, 0.7916666666666666297, 0.8020833333333333703, 0.8125000000000000000, 0.8229166666666666297, 0.8333333333333333703, 0.8437500000000000000, 0.8541666666666666297, 0.8645833333333333703, 0.8750000000000000000, 0.8854166666666666297, 0.8958333333333333703, 0.9062500000000000000, 0.9166666666666666297, 0.9270833333333333703, 0.9375000000000000000, 0.9479166666666666297, 0.9583333333333333703, 0.9687500000000000000, 0.9791666666666666297, 0.9895833333333333703, 1.000000000000000000 ),
 .UNSPECIFIED. ) 
 CURVE ( )  GEOMETRIC_REPRESENTATION_ITEM ( )  RATIONAL_B_SPLINE_CURVE ( ( 0.9869654386326103257, 0.9747051062697298374, 1.000000000000000000, 0.9659258262890683122, 1.000000000000000000, 0.9659258262890683122, 1.000000000000000000, 0.9659258262890683122, 1.000000000000000000, 0.9659258262890683122, 1.000000000000000000, 0.9659258262890683122, 1.000000000000000000, 0.9659258262890683122, 1.000000000000000000, 0.9659258262890683122, 1.000000000000000000, 0.9659258262890683122, 1.000000000000000000, 0.9659258262890683122, 1.000000000000000000, 0.9659258262890683122, 1.000000000000000000, 0.9659258262890683122, 1.000000000000000000, 0.9659258262890683122, 1.000000000000000000, 0.9659258262890683122, 1.000000000000000000, 0.9659258262890683122, 1.000000000000000000, 0.9659258262890683122, 1.000000000000000000, 0.9659258262890683122, 1.000000000000000000, 0.9659258262890683122, 1.000000000000000000, 0.9659258262890683122, 1.000000000000000000, 0.9659258262890683122, 1.000000000000000000, 0.9659258262890683122, 1.000000000000000000, 0.9659258262890683122, 1.000000000000000000, 0.9659258262890683122, 1.000000000000000000, 0.9659258262890683122, 1.000000000000000000, 0.9659258262890683122, 1.000000000000000000, 0.9659258262890683122, 1.000000000000000000, 0.9659258262890683122, 1.000000000000000000, 0.9659258262890683122, 1.000000000000000000, 0.9659258262890683122, 1.000000000000000000, 0.9659258262890683122, 1.000000000000000000, 0.9659258262890683122, 1.000000000000000000, 0.9659258262890683122, 1.000000000000000000, 0.9659258262890683122, 1.000000000000000000, 0.9659258262890683122, 1.000000000000000000, 0.9659258262890683122, 1.000000000000000000, 0.9659258262890683122, 1.000000000000000000, 0.9659258262890683122, 1.000000000000000000, 0.9659258262890683122, 1.000000000000000000, 0.9659258262890683122, 1.000000000000000000, 0.9659258262890683122, 1.000000000000000000, 0.9659258262890683122, 1.000000000000000000, 0.9659258262890683122, 1.000000000000000000, 0.9659258262890683122, 1.000000000000000000, 0.9659258262890683122, 1.000000000000000000, 0.9659258262890683122, 1.000000000000000000, 0.9659258262890683122, 1.000000000000000000, 0.9659258262890683122, 1.000000000000000000, 0.9659258262890683122, 1.000000000000000000, 0.9659258262890683122, 1.000000000000000000, 0.9659258262890683122, 1.000000000000000000, 0.9659258262890683122, 1.000000000000000000, 0.9659258262890683122, 1.000000000000000000, 0.9659258262890683122, 1.000000000000000000, 0.9659258262890683122, 1.000000000000000000, 0.9659258262890683122, 1.000000000000000000, 0.9659258262890683122, 1.000000000000000000, 0.9659258262890683122, 1.000000000000000000, 0.9659258262890683122, 1.000000000000000000, 0.9659258262890683122, 1.000000000000000000, 0.9659258262890683122, 1.000000000000000000, 0.9659258262890683122, 1.000000000000000000, 0.9659258262890683122, 1.000000000000000000, 0.9659258262890683122, 1.000000000000000000, 0.9659258262890683122, 1.000000000000000000, 0.9659258262890683122, 1.000000000000000000, 0.9659258262890683122, 1.000000000000000000, 0.9659258262890683122, 1.000000000000000000, 0.9659258262890683122, 1.000000000000000000, 0.9659258262890683122, 1.000000000000000000, 0.9659258262890683122, 1.000000000000000000, 0.9659258262890683122, 1.000000000000000000, 0.9659258262890683122, 1.000000000000000000, 0.9659258262890683122, 1.000000000000000000, 0.9659258262890683122, 1.000000000000000000, 0.9659258262890683122, 1.000000000000000000, 0.9659258262890683122, 1.000000000000000000, 0.9659258262890683122, 1.000000000000000000, 0.9659258262890683122, 1.000000000000000000, 0.9659258262890683122, 1.000000000000000000, 0.9659258262890683122, 1.000000000000000000, 0.9659258262890683122, 1.000000000000000000, 0.9659258262890683122, 1.000000000000000000, 0.9659258262890683122, 1.000000000000000000, 0.9659258262890683122, 1.000000000000000000, 0.9659258262890683122, 1.000000000000000000, 0.9659258262890683122, 1.000000000000000000, 0.9659258262890683122, 1.000000000000000000, 0.9659258262890683122, 1.000000000000000000, 0.9659258262890683122, 1.000000000000000000, 0.9659258262890683122, 1.000000000000000000, 0.9659258262890683122, 1.000000000000000000, 0.9659258262890683122, 1.000000000000000000, 0.9659258262890683122, 1.000000000000000000, 0.9659258262890683122, 1.000000000000000000 ) ) 
 REPRESENTATION_ITEM ( '' )  );
#236 = CARTESIAN_POINT ( 'NONE',  ( -41.00000000000000711, 53.00000000000000711, -45.00000000000000000 ) ) ;
#237 = DIRECTION ( 'NONE',  ( -0.7071067811865512365, -0.4999999999999988898, 0.4999999999999959477 ) ) ;
#238 = DIRECTION ( 'NONE',  ( 0.000000000000000000, -0.4999999999999992784, 0.8660254037844390407 ) ) ;
#239 = DIRECTION ( 'NONE',  ( 0.7071067811865513475, 0.4999999999999988898, -0.4999999999999959477 ) ) ;
#240 = CARTESIAN_POINT ( 'NONE',  ( -32.50000000000000000, 52.00000000000000711, 12.50000000000000000 ) ) ;
#241 = UNCERTAINTY_MEASURE_WITH_UNIT (LENGTH_MEASURE( 1.000000000000000082E-05 ), #5755, 'distance_accuracy_value', 'NONE');
#242 = EDGE_LOOP ( 'NONE', ( #10443, #19008, #2745 ) ) ;
#243 = DIRECTION ( 'NONE',  ( 6.123233995736766036E-17, -1.000000000000000000, 0.000000000000000000 ) ) ;
#244 = CARTESIAN_POINT ( 'NONE',  ( -13.82508104294698192, -29.04416526290806644, 11.91992750791695421 ) ) ;
#245 = CARTESIAN_POINT ( 'NONE',  ( -0.8996865886453131456, 66.25031470727165583, 44.99999999999998579 ) ) ;
#246 = CARTESIAN_POINT ( 'NONE',  ( -20.04416526290809131, -22.82508104294699791, 20.89257249208303691 ) ) ;
#247 = DIRECTION ( 'NONE',  ( 0.000000000000000000, 0.000000000000000000, 1.000000000000000000 ) ) ;
#248 = CARTESIAN_POINT ( 'NONE',  ( -10.75228648362910100, -26.64274437364854009, 11.26367750791695777 ) ) ;
#249 = LINE ( 'NONE', #3293, #1715 ) ;
#250 = CARTESIAN_POINT ( 'NONE',  ( -10.58745947852649927, -21.64274437364853654, 15.63867750791695777 ) ) ;
#251 = DIRECTION ( 'NONE',  ( -0.000000000000000000, -0.000000000000000000, -1.000000000000000000 ) ) ;
#252 = LINE ( 'NONE', #16158, #15418 ) ;
#253 = CARTESIAN_POINT ( 'NONE',  ( 2.066987300000001859, 64.85617417291294373, 46.20000000109247651 ) ) ;
#254 = CARTESIAN_POINT ( 'NONE',  ( -41.00000000000000711, 53.00000000000000711, 13.50000000000000000 ) ) ;
#255 = DIRECTION ( 'NONE',  ( 0.000000000000000000, 0.000000000000000000, -1.000000000000000000 ) ) ;
#256 = DIRECTION ( 'NONE',  ( 0.000000000000000000, 0.7071067811865490160, -0.7071067811865461294 ) ) ;
#257 = CARTESIAN_POINT ( 'NONE',  ( -2.066987300000001415, 63.14382582708705627, 47.40000000109247225 ) ) ;
#258 = EDGE_CURVE ( 'NONE', #10251, #6518, #1845, .T. ) ;
#259 = EDGE_CURVE ( 'NONE', #2631, #2004, #1460, .T. ) ;
#260 = PLANE ( 'NONE',  #8615 ) ;
#261 = ORIENTED_EDGE ( 'NONE', *, *, #4730, .T. ) ;
#262 = VERTEX_POINT ( 'NONE', #4895 ) ;
#263 = CARTESIAN_POINT ( 'NONE',  ( -14.83517299489734853, -30.99999999999998224, 19.36132249208304046 ) ) ;
#264 = CARTESIAN_POINT ( 'NONE',  ( -9.955834737091903364, -25.17491895705295235, 7.767572492083041347 ) ) ;
#265 = ORIENTED_EDGE ( 'NONE', *, *, #5234, .T. ) ;
#266 = CARTESIAN_POINT ( 'NONE',  ( -14.83517299489738761, -20.99999999999997513, 14.76367750791695954 ) ) ;
#267 = LINE ( 'NONE', #6253, #11429 ) ;
#268 = CARTESIAN_POINT ( 'NONE',  ( -7.999999999999996447, -23.83517299489733432, 18.04882249208304046 ) ) ;
#269 = FACE_OUTER_BOUND ( 'NONE', #16546, .T. ) ;
#270 = CARTESIAN_POINT ( 'NONE',  ( 2.066987300000001415, 64.00000000000000000, 47.55000000109247082 ) ) ;
#271 = ORIENTED_EDGE ( 'NONE', *, *, #18253, .T. ) ;
#272 = ORIENTED_EDGE ( 'NONE', *, *, #12825, .F. ) ;
#273 = AXIS2_PLACEMENT_3D ( 'NONE', #16902, #3471, #9445 ) ;
#274 = DIRECTION ( 'NONE',  ( -1.000000000000000000, 0.000000000000000000, 0.000000000000000000 ) ) ;
#275 = DIRECTION ( 'NONE',  ( 0.000000000000000000, 0.7071067811865456854, 0.7071067811865494601 ) ) ;
#276 = EDGE_CURVE ( 'NONE', #17921, #11844, #16850, .T. ) ;
#277 = ORIENTED_EDGE ( 'NONE', *, *, #8740, .F. ) ;
#278 = CARTESIAN_POINT ( 'NONE',  ( -2.066987300000000971, 63.14382582708704916, 48.00000000109246656 ) ) ;
#279 = CARTESIAN_POINT ( 'NONE',  ( -24.00000000000000711, 53.00000000000000711, -18.00000000000000000 ) ) ;
#280 = EDGE_CURVE ( 'NONE', #3613, #17642, #1950, .T. ) ;
#281 = LINE ( 'NONE', #12431, #10985 ) ;
#282 = CARTESIAN_POINT ( 'NONE',  ( 1.300000000000000044, 0.7390083445627193548, -1.280000000000000693 ) ) ;
#283 = AXIS2_PLACEMENT_3D ( 'NONE', #6653, #2040, #17044 ) ;
#284 = CARTESIAN_POINT ( 'NONE',  ( 14.99999999999998579, 3.000000000000000000, 26.99999999999997158 ) ) ;
#285 = EDGE_LOOP ( 'NONE', ( #7432, #10877, #13688, #10122 ) ) ;
#287 = EDGE_LOOP ( 'NONE', ( #9707, #2750, #19384, #14817 ) ) ;
#286 = ORIENTED_EDGE ( 'NONE', *, *, #17624, .F. ) ;
#288 = CARTESIAN_POINT ( 'NONE',  ( -11.64274437364854187, -30.14459132904234195, 16.95117750791695954 ) ) ;
#289 = VECTOR ( 'NONE', #11116, 1000.000000000000000 ) ;
#290 = EDGE_LOOP ( 'NONE', ( #1568, #17362, #14195, #8849 ) ) ;
#292 = VERTEX_POINT ( 'NONE', #6652 ) ;
#291 = VERTEX_POINT ( 'NONE', #667 ) ;
#293 = CARTESIAN_POINT ( 'NONE',  ( -14.83517299489736985, -26.99999999999998579, 14.11132249208304223 ) ) ;
#294 = CARTESIAN_POINT ( 'NONE',  ( -16.71081734191527346, -16.95583473709190159, 9.294927507916959541 ) ) ;
#295 = CARTESIAN_POINT ( 'NONE',  ( 2.066987300000001415, 64.85617417291294373, 49.20000000109247651 ) ) ;
#296 = CARTESIAN_POINT ( 'NONE',  ( 1.767766952966370653, 62.23223304703363112, 47.20000000218494307 ) ) ;
#297 = VERTEX_POINT ( 'NONE', #14188 ) ;
#298 = CARTESIAN_POINT ( 'NONE',  ( -16.35725562635142794, -21.31951028609535470, 14.32617750791695777 ) ) ;
#299 = AXIS2_PLACEMENT_3D ( 'NONE', #12287, #10903, #18180 ) ;
#300 = SURFACE_STYLE_USAGE ( .BOTH. , #13722 ) ;
#301 = VERTEX_POINT ( 'NONE', #18229 ) ;
#302 = ADVANCED_FACE ( 'NONE', ( #4804 ), #6459, .T. ) ;
#303 = EDGE_CURVE ( 'NONE', #628, #8146, #5681, .T. ) ;
#304 = LINE ( 'NONE', #9218, #18172 ) ;
#305 = ORIENTED_EDGE ( 'NONE', *, *, #2220, .F. ) ;
#306 =( NAMED_UNIT ( * ) PLANE_ANGLE_UNIT ( ) SI_UNIT ( $, .RADIAN. ) );
#307 = LINE ( 'NONE', #9221, #11899 ) ;
#308 = CARTESIAN_POINT ( 'NONE',  ( -3.155775640247338920, -41.39960408384398249, 3.000000000000000000 ) ) ;
#309 = LINE ( 'NONE', #12357, #13947 ) ;
#310 = VECTOR ( 'NONE', #16083, 1000.000000000000000 ) ;
#311 = DIRECTION ( 'NONE',  ( 1.000000000000000000, 0.000000000000000000, 0.000000000000000000 ) ) ;
#312 = ITEM_DEFINED_TRANSFORMATION ( 'NONE', 'NONE', #788,  #1791 ) ;
#313 = VECTOR ( 'NONE', #8610, 1000.000000000000000 ) ;
#314 = EDGE_CURVE ( 'NONE', #106, #11781, #3884, .T. ) ;
#315 = LINE ( 'NONE', #7965, #7095 ) ;
#316 = CARTESIAN_POINT ( 'NONE',  ( 2.500000000000001776, 64.00000000000000000, 46.50000000218494733 ) ) ;
#317 = DIRECTION ( 'NONE',  ( 0.000000000000000000, 0.000000000000000000, 1.000000000000000000 ) ) ;
#318 = AXIS2_PLACEMENT_3D ( 'NONE', #6383, #18632, #12346 ) ;
#319 = CARTESIAN_POINT ( 'NONE',  ( -40.00000000000000711, 110.0000000000000000, 30.00000000000000000 ) ) ;
#320 = ORIENTED_EDGE ( 'NONE', *, *, #11499, .F. ) ;
#321 = CARTESIAN_POINT ( 'NONE',  ( -13.82508104294698192, -29.04416526290806644, 11.91992750791695421 ) ) ;
#322 = VECTOR ( 'NONE', #8447, 1000.000000000000000 ) ;
#323 = CARTESIAN_POINT ( 'NONE',  ( -10.00000000000000000, 0.000000000000000000, 33.99999999999999289 ) ) ;
#324 = ORIENTED_EDGE ( 'NONE', *, *, #4947, .F. ) ;
#325 = CARTESIAN_POINT ( 'NONE',  ( -19.41254052147350961, -21.64274437364857562, 21.11132249208304401 ) ) ;
#326 = VECTOR ( 'NONE', #8831, 1000.000000000000000 ) ;
#327 = EDGE_CURVE ( 'NONE', #16495, #6094, #13076, .T. ) ;
#328 = CARTESIAN_POINT ( 'NONE',  ( -15.63902057219073605, -27.04416526290807710, 19.58007249208304046 ) ) ;
#329 = SURFACE_STYLE_USAGE ( .BOTH. , #10800 ) ;
#330 = EDGE_LOOP ( 'NONE', ( #1279, #8353, #4314, #6562 ) ) ;
#331 = AXIS2_PLACEMENT_3D ( 'NONE', #17063, #3625, #15585 ) ;
#332 = CARTESIAN_POINT ( 'NONE',  ( -25.00000000000000000, 113.0000000000000000, 30.00000000000000000 ) ) ;
#333 = ORIENTED_EDGE ( 'NONE', *, *, #12310, .F. ) ;
#334 = LINE ( 'NONE', #13649, #1223 ) ;
#335 = DIRECTION ( 'NONE',  ( -1.000000000000000000, 0.000000000000000000, 0.000000000000000000 ) ) ;
#336 = CARTESIAN_POINT ( 'NONE',  ( -1.084502282093227498E-14, 29.65425233947093986, 56.83102903476761725 ) ) ;
#337 = CARTESIAN_POINT ( 'NONE',  ( -15.00000000000001421, -18.99999999999997868, 42.00000000000000000 ) ) ;
#338 = VECTOR ( 'NONE', #15976, 1000.000000000000000 ) ;
#339 = DIRECTION ( 'NONE',  ( 0.000000000000000000, -1.000000000000000000, -0.000000000000000000 ) ) ;
#340 = DIRECTION ( 'NONE',  ( 1.000000000000000000, 0.000000000000000000, 0.000000000000000000 ) ) ;
#341 = DIRECTION ( 'NONE',  ( -0.000000000000000000, -1.000000000000000000, 0.000000000000000000 ) ) ;
#342 = AXIS2_PLACEMENT_3D ( 'NONE', #8168, #7978, #714 ) ;
#343 = EDGE_LOOP ( 'NONE', ( #9305, #13118, #10006, #16658 ) ) ;
#344 = DIRECTION ( 'NONE',  ( 0.000000000000000000, 0.000000000000000000, 1.000000000000000000 ) ) ;
#345 = AXIS2_PLACEMENT_3D ( 'NONE', #135, #15137, #1704 ) ;
#346 = CARTESIAN_POINT ( 'NONE',  ( -13.82508104294698192, -29.04416526290806644, 17.16992750791694888 ) ) ;
#347 = CARTESIAN_POINT ( 'NONE',  ( 2.500000000000001776, 64.00000000000000000, 46.50000000218494733 ) ) ;
#348 = CARTESIAN_POINT ( 'NONE',  ( -11.21908421996106320, -27.53959229564982181, 23.95507249208304401 ) ) ;
#349 = FACE_OUTER_BOUND ( 'NONE', #18147, .T. ) ;
#350 = CARTESIAN_POINT ( 'NONE',  ( -17.64274437364855430, -28.24771351637087236, 23.07617750791695954 ) ) ;
#351 = DIRECTION ( 'NONE',  ( 0.000000000000000000, 0.000000000000000000, 1.000000000000000000 ) ) ;
#352 = CARTESIAN_POINT ( 'NONE',  ( -14.83517299489739649, -18.99999999999997868, 14.76367750791695777 ) ) ;
#353 = DIRECTION ( 'NONE',  ( 1.000000000000000000, -0.000000000000000000, -0.000000000000000000 ) ) ;
#354 = FACE_OUTER_BOUND ( 'NONE', #14089, .T. ) ;
#355 =( GEOMETRIC_REPRESENTATION_CONTEXT ( 3 ) GLOBAL_UNCERTAINTY_ASSIGNED_CONTEXT ( ( #18086 ) ) GLOBAL_UNIT_ASSIGNED_CONTEXT ( ( #12843, #5500, #19029 ) ) REPRESENTATION_CONTEXT ( 'NONE', 'WORKASPACE' ) );
#356 = CARTESIAN_POINT ( 'NONE',  ( -2.066987300000001415, 63.14382582708705627, 48.20000000109247651 ) ) ;
#357 = CARTESIAN_POINT ( 'NONE',  ( -4.189607678530257395, 32.40336399182267257, 53.72836399182263278 ) ) ;
#358 = DIRECTION ( 'NONE',  ( 1.000000000000000000, -0.000000000000000000, -0.000000000000000000 ) ) ;
#359 = VECTOR ( 'NONE', #18061, 1000.000000000000000 ) ;
#360 = CARTESIAN_POINT ( 'NONE',  ( -1.265664690411616068E-16, 66.06698730000000808, 46.35000000109246798 ) ) ;
#361 = CARTESIAN_POINT ( 'NONE',  ( -41.00000000000000711, 53.00000000000000711, 27.50000000000000000 ) ) ;
#362 = AXIS2_PLACEMENT_3D ( 'NONE', #17371, #11102, #3758 ) ;
#363 = EDGE_LOOP ( 'NONE', ( #16148, #12127, #5971, #7441 ) ) ;
#364 = ORIENTED_EDGE ( 'NONE', *, *, #7937, .T. ) ;
#365 = CARTESIAN_POINT ( 'NONE',  ( -9.020235676060250896, -20.35725562635137820, 38.61132249208304046 ) ) ;
#366 = VECTOR ( 'NONE', #8391, 1000.000000000000000 ) ;
#367 = CARTESIAN_POINT ( 'NONE',  ( -12.64274437364858628, -19.58745947852646552, 6.673822492083040459 ) ) ;
#368 = ORIENTED_EDGE ( 'NONE', *, *, #14861, .F. ) ;
#369 = CARTESIAN_POINT ( 'NONE',  ( -16.64274437364856496, -26.51566270880199738, 23.07617750791695954 ) ) ;
#370 = LINE ( 'NONE', #15368, #6453 ) ;
#371 = CARTESIAN_POINT ( 'NONE',  ( -21.95583473709189803, -26.04047135212049469, 15.20507249208304046 ) ) ;
#372 = VECTOR ( 'NONE', #7310, 1000.000000000000000 ) ;
#373 = CARTESIAN_POINT ( 'NONE',  ( -2.500000000000001776, 64.00000000000000000, 48.39999999999999858 ) ) ;
#374 = CARTESIAN_POINT ( 'NONE',  ( 3.796994071234847710E-16, 61.93301269999999903, 47.35000000109246798 ) ) ;
#375 = VERTEX_POINT ( 'NONE', #7113 ) ;
#376 = ORIENTED_EDGE ( 'NONE', *, *, #4655, .F. ) ;
#377 = EDGE_CURVE ( 'NONE', #14750, #2431, #8581, .T. ) ;
#378 = ADVANCED_FACE ( 'NONE', ( #14562 ), #11224, .T. ) ;
#379 = CARTESIAN_POINT ( 'NONE',  ( -25.00000000000000000, 53.00000000000000711, 30.00000000000000000 ) ) ;
#380 = DIRECTION ( 'NONE',  ( -0.000000000000000000, -0.000000000000000000, -1.000000000000000000 ) ) ;
#381 = ORIENTED_EDGE ( 'NONE', *, *, #2414, .F. ) ;
#382 = CARTESIAN_POINT ( 'NONE',  ( -2.066987300000001415, 64.85617417291294373, 49.50000000109246656 ) ) ;
#383 = DIRECTION ( 'NONE',  ( -1.000000000000000000, -0.000000000000000000, -0.000000000000000000 ) ) ;
#384 = EDGE_CURVE ( 'NONE', #16449, #5562, #9851, .T. ) ;
#385 = CARTESIAN_POINT ( 'NONE',  ( 0.8561741729129460632, 66.06698729999999387, 45.50000000109247367 ) ) ;
#386 = DIRECTION ( 'NONE',  ( 0.000000000000000000, 0.7071067811865456854, 0.7071067811865494601 ) ) ;
#387 = EDGE_CURVE ( 'NONE', #7750, #14031, #2123, .T. ) ;
#388 = CARTESIAN_POINT ( 'NONE',  ( 2.500000000000001776, 64.00000000000000000, 47.30000000218494449 ) ) ;
#389 = EDGE_LOOP ( 'NONE', ( #6259, #18026, #496, #1957 ) ) ;
#391 = EDGE_LOOP ( 'NONE', ( #18321, #5980, #17279, #6106, #2334 ) ) ;
#390 = EDGE_LOOP ( 'NONE', ( #5193, #765, #2617, #19104 ) ) ;
#392 = CARTESIAN_POINT ( 'NONE',  ( -8.855408670957631401, -20.64274437364852943, 26.13867750791696309 ) ) ;
#393 = VECTOR ( 'NONE', #11200, 1000.000000000000000 ) ;
#394 = EDGE_LOOP ( 'NONE', ( #6539, #4312, #7875, #13610 ) ) ;
#395 = EDGE_LOOP ( 'NONE', ( #10179, #10468 ) ) ;
#396 = CARTESIAN_POINT ( 'NONE',  ( -14.03132541760400009, -26.95583473709189448, 13.89257249208304401 ) ) ;
#397 = CARTESIAN_POINT ( 'NONE',  ( -8.044165262908075320, -26.04047135212042718, 11.04492750791695777 ) ) ;
#398 = AXIS2_PLACEMENT_3D ( 'NONE', #14982, #7531, #3118 ) ;
#399 = CARTESIAN_POINT ( 'NONE',  ( -0.8561741729129466183, 61.93301270000000613, 47.30000000109247082 ) ) ;
#400 = FACE_OUTER_BOUND ( 'NONE', #585, .T. ) ;
#401 = ORIENTED_EDGE ( 'NONE', *, *, #9823, .T. ) ;
#402 = CARTESIAN_POINT ( 'NONE',  ( -12.04416526290807887, -24.96867458239596260, 11.04492750791696132 ) ) ;
#403 =( LENGTH_UNIT ( ) NAMED_UNIT ( * ) SI_UNIT ( .MILLI., .METRE. ) );
#404 = ORIENTED_EDGE ( 'NONE', *, *, #14193, .T. ) ;
#405 = CARTESIAN_POINT ( 'NONE',  ( 2.500000000000001776, 64.00000000000000000, 45.59999999999999432 ) ) ;
#406 = ORIENTED_EDGE ( 'NONE', *, *, #3062, .T. ) ;
#407 = DIRECTION ( 'NONE',  ( -0.000000000000000000, -1.000000000000000000, -0.000000000000000000 ) ) ;
#408 = LINE ( 'NONE', #5209, #9039 ) ;
#409 = DIRECTION ( 'NONE',  ( 1.000000000000000000, -0.000000000000000000, -0.000000000000000000 ) ) ;
#410 = CARTESIAN_POINT ( 'NONE',  ( 0.8561741729129472844, 61.93301270000000613, 48.20000000109248361 ) ) ;
#411 = PLANE ( 'NONE',  #5533 ) ;
#412 = CARTESIAN_POINT ( 'NONE',  ( -41.00000000000000711, 53.00000000000000711, 6.999999999999999112 ) ) ;
#413 = CARTESIAN_POINT ( 'NONE',  ( 43.50000000000001421, 118.0000000000000142, 32.49999999999998579 ) ) ;
#414 = CARTESIAN_POINT ( 'NONE',  ( -15.20357423236093375, -43.78611686177728046, 3.000000000000000000 ) ) ;
#415 = ORIENTED_EDGE ( 'NONE', *, *, #7089, .T. ) ;
#416 = CARTESIAN_POINT ( 'NONE',  ( -19.99999999999999645, -23.83517299489738051, 13.45117750791695777 ) ) ;
#417 = DIRECTION ( 'NONE',  ( -0.000000000000000000, 1.000000000000000000, -0.000000000000000000 ) ) ;
#418 = ADVANCED_FACE ( 'NONE', ( #11608 ), #4181, .T. ) ;
#419 = ORIENTED_EDGE ( 'NONE', *, *, #16592, .T. ) ;
#420 = EDGE_CURVE ( 'NONE', #9430, #8882, #10133, .T. ) ;
#421 = UNCERTAINTY_MEASURE_WITH_UNIT (LENGTH_MEASURE( 1.000000000000000082E-05 ), #7921, 'distance_accuracy_value', 'NONE');
#422 = CARTESIAN_POINT ( 'NONE',  ( -10.75228648362912232, -21.35725562635138530, 22.86132249208304401 ) ) ;
#423 = EDGE_CURVE ( 'NONE', #13623, #11742, #14277, .T. ) ;
#424 = CARTESIAN_POINT ( 'NONE',  ( -11.95583473709190514, -24.63902057219072361, 18.26757249208304401 ) ) ;
#425 = CARTESIAN_POINT ( 'NONE',  ( -43.50000000000000000, 115.0000000000000000, 32.50000000000000000 ) ) ;
#426 = EDGE_LOOP ( 'NONE', ( #14874, #12807, #12078, #5130, #11922 ) ) ;
#427 = CARTESIAN_POINT ( 'NONE',  ( 0.2500000000000002220, 4.898587196589412829E-16, -4.000000000000000000 ) ) ;
#428 = VERTEX_POINT ( 'NONE', #16040 ) ;
#429 = LINE ( 'NONE', #4946, #12185 ) ;
#430 = CARTESIAN_POINT ( 'NONE',  ( -41.00000000000000711, 110.0000000000000000, -6.000000000000001776 ) ) ;
#431 = LINE ( 'NONE', #5236, #10029 ) ;
#432 = DIRECTION ( 'NONE',  ( 1.000000000000000000, -0.000000000000000000, -0.000000000000000000 ) ) ;
#433 = ADVANCED_FACE ( 'NONE', ( #10043 ), #844, .T. ) ;
#434 = DIRECTION ( 'NONE',  ( -0.000000000000000000, 1.000000000000000000, -0.000000000000000000 ) ) ;
#435 =( REPRESENTATION_RELATIONSHIP ('NONE','NONE', #7912, #12005 ) REPRESENTATION_RELATIONSHIP_WITH_TRANSFORMATION ( #15746 )SHAPE_REPRESENTATION_RELATIONSHIP( ) );
#436 = EDGE_CURVE ( 'NONE', #19394, #6733, #8675, .T. ) ;
#437 = CARTESIAN_POINT ( 'NONE',  ( -41.00000000000000711, 110.0000000000000000, 20.00000000000000000 ) ) ;
#438 = CARTESIAN_POINT ( 'NONE',  ( -2.500000000000001776, 64.00000000000000000, 47.70000000218494307 ) ) ;
#439 = UNCERTAINTY_MEASURE_WITH_UNIT (LENGTH_MEASURE( 1.000000000000000082E-05 ), #14477, 'distance_accuracy_value', 'NONE');
#440 = ORIENTED_EDGE ( 'NONE', *, *, #14376, .F. ) ;
#441 = CARTESIAN_POINT ( 'NONE',  ( -10.58745947852649927, -21.64274437364853654, 20.88867750791695954 ) ) ;
#442 = CARTESIAN_POINT ( 'NONE',  ( 2.500000000000001776, 64.00000000000000000, 47.30000000218494449 ) ) ;
#443 = CARTESIAN_POINT ( 'NONE',  ( -17.35725562635140307, -28.41254052147349185, 19.79882249208304046 ) ) ;
#444 = DIRECTION ( 'NONE',  ( -0.000000000000000000, -0.000000000000000000, -1.000000000000000000 ) ) ;
#445 = CARTESIAN_POINT ( 'NONE',  ( -18.53959229564986799, -20.21908421996107563, 14.10742750791695777 ) ) ;
#446 = DIRECTION ( 'NONE',  ( -1.000000000000000000, 0.000000000000000000, -0.000000000000000000 ) ) ;
#447 = CARTESIAN_POINT ( 'NONE',  ( -15.16482700510259640, -28.99999999999998224, 22.63867750791695954 ) ) ;
#448 = CARTESIAN_POINT ( 'NONE',  ( -41.99999999999997868, 6.000000000000005329, 51.99999999999997868 ) ) ;
#449 = CARTESIAN_POINT ( 'NONE',  ( -18.78091578003892792, -20.46040770435013556, 31.83007249208304046 ) ) ;
#450 = CARTESIAN_POINT ( 'NONE',  ( 1.461580736456473684, 65.46158073645646880, 48.65000000109247225 ) ) ;
#451 = DIRECTION ( 'NONE',  ( 1.000000000000000000, 0.000000000000000000, 0.000000000000000000 ) ) ;
#452 = LINE ( 'NONE', #1930, #15081 ) ;
#453 = ADVANCED_FACE ( 'NONE', ( #1229 ), #11327, .T. ) ;
#454 = CYLINDRICAL_SURFACE ( 'NONE', #225, 2.999999999999999112 ) ;
#455 = CARTESIAN_POINT ( 'NONE',  ( -1.461580736456473906, 65.46158073645646880, 48.05000000109247082 ) ) ;
#456 = DIRECTION ( 'NONE',  ( -0.000000000000000000, -0.000000000000000000, -1.000000000000000000 ) ) ;
#457 = VECTOR ( 'NONE', #7788, 1000.000000000000000 ) ;
#458 = EDGE_LOOP ( 'NONE', ( #8935, #13551, #15098, #14265 ) ) ;
#459 = ORIENTED_EDGE ( 'NONE', *, *, #7687, .F. ) ;
#460 = CARTESIAN_POINT ( 'NONE',  ( -11.35725562635139418, -29.97976432393972601, 29.42382249208304046 ) ) ;
#461 = CARTESIAN_POINT ( 'NONE',  ( -18.53959229564983247, -27.78091578003891016, 9.517572492083040459 ) ) ;
#462 = ORIENTED_EDGE ( 'NONE', *, *, #8308, .F. ) ;
#463 = CARTESIAN_POINT ( 'NONE',  ( -16.64274437364856496, -26.51566270880199738, 33.57617750791696665 ) ) ;
#464 = DIRECTION ( 'NONE',  ( 0.000000000000000000, -1.000000000000000000, 0.000000000000000000 ) ) ;
#465 = CARTESIAN_POINT ( 'NONE',  ( -12.95952864787948755, -30.95583473709188382, 24.39257249208303691 ) ) ;
#466 = CARTESIAN_POINT ( 'NONE',  ( 1.461580736456473684, 65.46158073645646880, 45.25000000109247367 ) ) ;
#467 = CARTESIAN_POINT ( 'NONE',  ( -2.066987300000001859, 64.85617417291294373, 47.90000000109247225 ) ) ;
#468 = ORIENTED_EDGE ( 'NONE', *, *, #1195, .F. ) ;
#469 = ORIENTED_EDGE ( 'NONE', *, *, #9014, .T. ) ;
#470 = CARTESIAN_POINT ( 'NONE',  ( -2.500000000000011546, 65.03553390593272354, 46.05000000218494449 ) ) ;
#471 = DIRECTION ( 'NONE',  ( 0.000000000000000000, -1.000000000000000000, 0.000000000000000000 ) ) ;
#472 = VECTOR ( 'NONE', #8947, 1000.000000000000000 ) ;
#473 = CARTESIAN_POINT ( 'NONE',  ( 3.796994071234847710E-16, 61.93301269999999903, 48.95000000109246940 ) ) ;
#474 = DIRECTION ( 'NONE',  ( 0.000000000000000000, 0.000000000000000000, 1.000000000000000000 ) ) ;
#475 = DIRECTION ( 'NONE',  ( -0.7071067811865511255, -0.4999999999999987788, 0.4999999999999958922 ) ) ;
#476 = EDGE_CURVE ( 'NONE', #18462, #4631, #2600, .T. ) ;
#477 = EDGE_CURVE ( 'NONE', #3996, #8594, #18791, .T. ) ;
#478 = LINE ( 'NONE', #15666, #7219 ) ;
#479 = DIRECTION ( 'NONE',  ( -0.000000000000000000, -1.000000000000000000, -0.000000000000000000 ) ) ;
#480 = ORIENTED_EDGE ( 'NONE', *, *, #9077, .T. ) ;
#482 = ORIENTED_EDGE ( 'NONE', *, *, #8871, .F. ) ;
#481 = EDGE_LOOP ( 'NONE', ( #15484, #1248, #5355, #15133 ) ) ;
#483 = CARTESIAN_POINT ( 'NONE',  ( -8.044165262908075320, -26.04047135212042718, 32.04492750791695954 ) ) ;
#484 = PRODUCT_DEFINITION_FORMATION_WITH_SPECIFIED_SOURCE ( 'ANY', '', #8955, .NOT_KNOWN. ) ;
#485 = ORIENTED_EDGE ( 'NONE', *, *, #2062, .T. ) ;
#486 = VECTOR ( 'NONE', #10587, 1000.000000000000000 ) ;
#487 = ORIENTED_EDGE ( 'NONE', *, *, #6763, .T. ) ;
#488 = CARTESIAN_POINT ( 'NONE',  ( -15.63902057219073605, -27.04416526290807710, 24.83007249208304046 ) ) ;
#489 = CARTESIAN_POINT ( 'NONE',  ( -13.28918265808472299, -31.04416526290805933, 17.16992750791696309 ) ) ;
#490 = CARTESIAN_POINT ( 'NONE',  ( -2.066987300000001415, 64.00000000000000000, 49.55000000109247082 ) ) ;
#491 = DIRECTION ( 'NONE',  ( -1.000000000000000000, -0.000000000000000000, -0.000000000000000000 ) ) ;
#492 = ORIENTED_EDGE ( 'NONE', *, *, #2758, .T. ) ;
#493 = CARTESIAN_POINT ( 'NONE',  ( -14.03132541760401786, -21.04416526290806289, 20.23242750791696309 ) ) ;
#494 = ORIENTED_EDGE ( 'NONE', *, *, #810, .F. ) ;
#495 = CARTESIAN_POINT ( 'NONE',  ( -50.00000000000001421, 17.99999999999993250, 59.99999999999997868 ) ) ;
#496 = ORIENTED_EDGE ( 'NONE', *, *, #14059, .F. ) ;
#497 = DIRECTION ( 'NONE',  ( -1.000000000000000000, 0.000000000000000000, -9.251858538542970348E-17 ) ) ;
#498 = DIRECTION ( 'NONE',  ( 1.000000000000000000, 0.000000000000000000, -0.000000000000000000 ) ) ;
#499 = CARTESIAN_POINT ( 'NONE',  ( -25.00000000000000711, 53.00000000000000711, 1.500000000000001332 ) ) ;
#500 = EDGE_CURVE ( 'NONE', #10686, #11531, #674, .T. ) ;
#501 = FACE_BOUND ( 'NONE', #14667, .T. ) ;
#502 = AXIS2_PLACEMENT_3D ( 'NONE', #7049, #17444, #4014 ) ;
#503 = LINE ( 'NONE', #18262, #13813 ) ;
#504 = CIRCLE ( 'NONE', #4888, 1.280000000000000027 ) ;
#505 = CARTESIAN_POINT ( 'NONE',  ( -1.767766952966370209, 65.76776695296638309, 49.20000000218494307 ) ) ;
#506 = CARTESIAN_POINT ( 'NONE',  ( -41.00000000000000711, 53.00000000000000711, -45.00000000000000000 ) ) ;
#507 = DIRECTION ( 'NONE',  ( 0.000000000000000000, -1.000000000000000000, 0.000000000000000000 ) ) ;
#508 = CARTESIAN_POINT ( 'NONE',  ( 20.00000000000000355, -32.00000000000000711, 1.500000000000000000 ) ) ;
#509 = ORIENTED_EDGE ( 'NONE', *, *, #2274, .F. ) ;
#510 = EDGE_CURVE ( 'NONE', #15185, #7828, #9171, .T. ) ;
#511 = CARTESIAN_POINT ( 'NONE',  ( -10.75228648362910100, -26.64274437364854009, 27.01367750791695954 ) ) ;
#512 = CARTESIAN_POINT ( 'NONE',  ( -41.00000000000000711, 53.00000000000000711, 26.50000000000000000 ) ) ;
#513 = VERTEX_POINT ( 'NONE', #10239 ) ;
#514 = CARTESIAN_POINT ( 'NONE',  ( -19.99999999999999645, -24.16482700510261949, 31.17382249208304046 ) ) ;
#515 = AXIS2_PLACEMENT_3D ( 'NONE', #7618, #13582, #166 ) ;
#516 = VECTOR ( 'NONE', #18188, 1000.000000000000000 ) ;
#517 = CARTESIAN_POINT ( 'NONE',  ( -11.95583473709190514, -24.63902057219072361, 23.51757249208304401 ) ) ;
#518 =( BOUNDED_SURFACE ( )  B_SPLINE_SURFACE ( 3, 2, ( 
 ( #10197, #8455, #1007, #8641, #5511, #1394, #8550, #16095, #7170, #18945, #11476, #16192, #7369, #4038, #13143, #17663, #4241, #14624, #5610, #1301, #10003, #13339, #19237, #13041, #2466, #2757, #16287, #17570, #11770, #14826, #4148, #16007, #19338, #10099, #2567, #14524, #10294, #11867, #9911, #1095, #14431, #14723, #17765, #17867, #7276, #13241, #5804, #2861, #15904, #18066, #15222, #7670, #9231, #7571, #4441, #6403, #13542, #16590, #18166, #321, #14925, #4838, #6304, #4741, #17965, #4641, #416, #120, #12368, #9326, #6104, #20, #1790, #1597, #16393, #18270, #10399, #12068, #12274, #13738, #3158, #10594, #3259, #9138, #13436, #15021, #10791, #3361, #7773, #16790, #2957, #12167, #6009, #15122, #8933, #7467, #13843, #16695, #7876, #1690, #15313, #13637, #1498, #222, #11971, #6207, #4539, #10699, #1891, #10495, #16492, #3056, #9032, #17174, #603, #18655, #16887, #9427, #17082, #13938, #9800, #16993, #5131, #9616, #15422, #1986, #5220, #15794, #511, #15602, #14133, #8160, #11084, #8071, #9709, #12461, #2360, #8257, #15509, #10892, #6688, #5306, #14032, #794, #3834, #6596, #6498, #8343, #2082, #18459, #5029, #12744, #14315, #18366, #10989, #3453, #3552, #6779, #882, #2171, #3736, #708, #7970, #12566, #18563, #15702, #12654, #2271, #3644, #4935, #6861, #11174, #14225, #18740, #11266, #9520, #17267, #14502, #1275, #14698, #19022, #1074, #1373, #14604, #5587, #13022, #17447, #16264, #7254, #4017, #18923, #5690, #2634 ),
 ( #13221, #4123, #17544, #5781, #7053, #11650, #8528, #9979, #11549, #2836, #14406, #10079, #16073, #8819, #14805, #12835, #19118, #8620, #5405, #17353, #8710, #19213, #1171, #11743, #2446, #7149, #15983, #17640, #17740, #13119, #18833, #4216, #8430, #10171, #4315, #10271, #16170, #983, #11360, #2739, #3924, #9892, #15885, #6959, #12929, #5492, #11455, #2545, #16763, #6185, #18136, #3130, #16371, #16564, #7645, #16668, #14993, #3032, #1570, #10762, #1671, #9109, #15099, #13612, #12044, #15287, #17841, #9009, #198, #7544, #7748, #13519, #7342, #3233, #16467, #98, #6080, #4415, #4714, #4814, #10668, #12142, #288, #19313, #15194, #3335, #1765, #10377, #9206, #18239, #7443, #5982, #13410, #10570, #13712, #6274, #18043, #4616, #12244, #9303, #13313, #11841, #5880, #2935, #8910, #14899, #1474, #6085, #11951, #17943, #4515, #10472, #9584, #16964, #10866, #12437, #17143, #764, #679, #9679, #13811, #15577, #16861, #14003, #392, #4908, #11234, #14103, #5275, #2047, #6745, #15481, #3807, #8042, #7847, #5102, #15391, #10960, #2241, #18534, #1959, #3706, #15672, #6662, #3526, #2144, #6375, #12338, #575, #3423, #12716, #483, #6564, #12533, #18336, #9396, #8131, #18713, #7945, #11056, #17052, #3615, #12627, #9492, #18622, #13905, #17239, #11148, #18433, #6470, #5187, #8232, #14197, #9773, #1860, #5002, #3895, #13194, #18900, #17328, #15860, #10143, #11716, #15768, #9862, #14287, #2419, #17613, #17710, #18995, #1146, #11518, #5378 ),
 ( #2331, #4291, #14476, #5463, #2608, #12991, #8314, #9950, #17422, #4190, #16142, #2515, #3992, #855, #17511, #11426, #8499, #10052, #11622, #6834, #2712, #8685, #16048, #8402, #15950, #12803, #1047, #18803, #1243, #7024, #11336, #13089, #12903, #14375, #14668, #951, #5560, #7223, #5659, #4090, #8592, #14573, #6933, #7123, #19089, #19187, #5754, #6154, #1346, #10641, #12116, #4586, #4389, #10445, #6247, #5953, #18216, #15169, #13386, #5856, #7621, #7419, #2808, #4683, #16235, #11924, #18110, #170, #3002, #19381, #9085, #17918, #19284, #1442, #16644, #9183, #15073, #3209, #8786, #18013, #11817, #8982, #14777, #13283, #263, #3102, #13685, #16437, #1737, #4491, #12214, #14969, #7317, #13492, #10347, #1542, #7720, #7517, #16345, #10248, #17812, #1648, #74, #10545, #2909, #8883, #6054, #14870, #12016, #16535, #13585, #15457, #1834, #7815, #11033, #2470, #6353, #2026, #554, #13982, #16936, #13884, #15555, #18312, #8460, #14078, #1937, #16738, #12506, #11127, #460, #6642, #9657, #6445, #12316, #14435, #7920, #4880, #10840, #18599, #1010, #4792, #16835, #3307, #3400, #12606, #6985, #8016, #9562, #6541, #13785, #18410, #4977, #2125, #18509, #8109, #12412, #10741, #12951, #3501, #10935, #17033, #5076, #9276, #9471, #3591, #5166, #17123, #651, #3687, #15647, #15265, #365, #9367, #15361, #17667, #8646, #5809, #16195, #5517, #13148, #1192, #7373, #1398, #5717, #7174, #7470, #1305, #2664, #11676, #13244, #14829, #10007 ),
 ( #8936, #17768, #10298, #14727, #8553, #8735, #19241, #8844, #19145, #14628, #4244, #2960, #11776, #7279, #4342, #16292, #10204, #18949, #16012, #2762, #2864, #13347, #19341, #5907, #11479, #11872, #17871, #4444, #10402, #2571, #16396, #14931, #1503, #17467, #4042, #14528, #1098, #7081, #13044, #19043, #5614, #11577, #17574, #4153, #10103, #16099, #6308, #12279, #7674, #4747, #9234, #10796, #16698, #17968, #16891, #16793, #4841, #12372, #7575, #18370, #9141, #1602, #9432, #3365, #1795, #226, #13640, #18071, #3457, #7880, #4644, #123, #18274, #3263, #7776, #6406, #6210, #3163, #12171, #15425, #13846, #10702, #18171, #4940, #15126, #9329, #1693, #10598, #15225, #1989, #15026, #13741, #325, #13440, #25, #6012, #15316, #1894, #11974, #4542, #422, #13545, #10498, #10897, #16498, #3060, #9038, #16595, #6108, #12071, #18566, #14036, #797, #17177, #2275, #886, #8164, #17085, #6691, #3927, #2363, #18658, #12658, #6866, #9620, #6782, #3649, #5134, #5223, #17358, #9524, #15606, #711, #9895, #11363, #15888, #14229, #3740, #514, #12464, #3838, #8346, #11179, #14318, #16996, #9713, #11088, #12748, #12838, #15706, #7975, #18745, #3555, #5309, #18838, #5408, #8261, #15514, #13941, #17271, #11270, #6503, #9804, #18464, #2085, #5033, #10994, #8074, #606, #15798, #6602, #12570, #2174, #14137, #2743, #11747, #10083, #17548, #16076, #5885, #16174, #4221, #10176, #8715, #7153, #10382, #12932, #4128, #14702, #2640, #2841, #8623, #2450 ),
 ( #19317, #5787, #1280, #14809, #14411, #10276, #11846, #16269, #5495, #4319, #13318, #2550, #1078, #8532, #5695, #7258, #13225, #14607, #13122, #17645, #19217, #11654, #6963, #17846, #17745, #8824, #1377, #15987, #7348, #8433, #4420, #11552, #1174, #19122, #18927, #987, #11458, #17450, #4021, #9982, #14506, #7056, #13025, #19025, #5591, #18244, #7851, #16471, #14998, #3036, #202, #9209, #15201, #10574, #7650, #12146, #13716, #6189, #1478, #396, #293, #7751, #15292, #10478, #1865, #12050, #4519, #12342, #6278, #4718, #3135, #16569, #1575, #6378, #10765, #7549, #9013, #1769, #18141, #10673, #9307, #9114, #6084, #15104, #18341, #16768, #13616, #1674, #13817, #18048, #12248, #4621, #13524, #16674, #4911, #17947, #3237, #4818, #16375, #2939, #8915, #3339, #14903, #7447, #13415, #1, #5987, #11956, #103, #488, #12631, #2053, #17148, #5279, #6666, #18809, #9685, #6474, #8236, #3812, #15772, #14109, #12441, #859, #768, #15677, #10870, #2247, #14292, #18437, #3428, #6838, #5006, #12809, #14202, #6752, #18627, #10964, #684, #11152, #12720, #18538, #6572, #5106, #16865, #5194, #3711, #18717, #11239, #15581, #9400, #1962, #12538, #17243, #11060, #9779, #17056, #2335, #8321, #16969, #15395, #7948, #13909, #3529, #9496, #15485, #8046, #14008, #579, #3621, #9589, #2148, #8136, #1151, #14382, #14580, #5664, #14674, #12999, #1052, #19000, #8793, #19094, #7128, #13094, #11628, #10057, #13288, #15864, #7029, #17618, #5565, #5759 ),
 ( #2424, #16149, #2814, #8691, #4195, #17718, #17333, #13198, #14782, #19192, #8407, #7229, #16241, #5468, #3997, #11433, #8596, #10147, #2718, #11523, #16052, #1249, #11721, #4295, #9869, #1351, #10252, #7323, #5383, #18904, #11341, #17517, #12908, #3900, #956, #6938, #4097, #2612, #9955, #17426, #15957, #2522, #8503, #14481, #9089, #13590, #12218, #79, #8987, #18018, #15268, #13690, #10551, #4593, #18219, #1548, #18116, #14974, #16442, #16540, #9282, #1450, #7523, #12022, #1837, #3311, #7821, #6161, #15078, #11821, #4395, #15175, #266, #3108, #6252, #8888, #1652, #10450, #12121, #4796, #7626, #19291, #4688, #14876, #16649, #10745, #6059, #13497, #5861, #175, #3010, #10646, #3214, #1742, #10355, #16742, #7727, #9187, #13390, #17817, #16349, #2914, #7423, #19386, #5959, #11930, #17923, #4495, #6357, #8213, #369, #9474, #2221, #3689, #6545, #3505, #12609, #15460, #3403, #4982, #9659, #12695, #18603, #14181, #12320, #2127, #9372, #12512, #18316, #16841, #3790, #6644, #17221, #13987, #18699, #8020, #15750, #557, #4884, #17036, #7924, #2029, #746, #11037, #13887, #15651, #6728, #5168, #18513, #14082, #10846, #15367, #5080, #1940, #5261, #12418, #3593, #9564, #463, #6449, #657, #11215, #18415, #15559, #8111, #11129, #17127, #9757, #2312, #10939, #13789, #16942, #5448, #838, #16034, #14650, #3976, #10126, #13174, #9933, #15839, #5739, #11407, #9843, #8385, #2692, #4270, #8296, #2403, #6819, #14358, #16123, #10232 ),
 ( #12786, #18783, #4175, #8668, #7008, #1220, #17313, #10036, #18886, #14554, #7202, #4068, #16216, #7106, #3876, #19168, #15930, #13069, #2496, #17402, #12976, #17692, #933, #8483, #1033, #14268, #11699, #5359, #1125, #2593, #11319, #6914, #12887, #14460, #18975, #5545, #11501, #8575, #17491, #19067, #5640, #11601, #17598, #17992, #5836, #16518, #146, #12093, #14952, #11800, #10620, #9062, #4566, #9162, #10523, #4663, #17794, #8765, #16621, #4367, #3188, #3081, #15050, #7494, #19267, #1525, #6037, #1628, #5930, #13370, #11901, #2787, #11994, #7598, #13565, #6131, #8962, #14755, #10327, #17899, #18091, #10422, #1329, #16417, #7299, #13266, #13470, #16324, #53, #19362, #2891, #8866, #14851, #1424, #7399, #2982, #4471, #4336, #14719, #3942, #2755, #11766, #1002, #18942, #6978, #4146, #13140, #19139, #14520, #11569, #16090, #17660, #10097, #5421, #10292, #4237, #11670, #19234, #14428, #5803, #16005, #8452, #16285, #10195, #8639, #7073, #1093, #5508, #2858, #1299, #11473, #12944, #5712, #2658, #14622, #13239, #13039, #10000, #19037, #8838, #7274, #17567, #5608, #900, #17763, #4035, #15900, #16190, #17462, #12854, #6881, #18856, #11377, #1187, #7168, #8729, #17369, #9908, #2464, #2565, #8546, #16588, #9030, #15219, #15017, #3358, #10694, #4536, #7569, #16490, #11865, #6205, #12271, #18163, #3154, #7770, #7367, #3256, #18265, #9227, #17865, #16691, #6301, #14923, #13433, #1496, #18064, #7667, #13635, #1594, #6101, #10592, #12164 ) ),
 .UNSPECIFIED., .T., .F., .F. ) 
 B_SPLINE_SURFACE_WITH_KNOTS ( ( 4, 3, 4 ),
 ( 3, 2, 2, 2, 2, 2, 2, 2, 2, 2, 2, 2, 2, 2, 2, 2, 2, 2, 2, 2, 2, 2, 2, 2, 2, 2, 2, 2, 2, 2, 2, 2, 2, 2, 2, 2, 2, 2, 2, 2, 2, 2, 2, 2, 2, 2, 2, 2, 2, 2, 2, 2, 2, 2, 2, 2, 2, 2, 2, 2, 2, 2, 2, 2, 2, 2, 2, 2, 2, 2, 2, 2, 2, 2, 2, 2, 2, 2, 2, 2, 2, 2, 2, 2, 2, 2, 2, 2, 2, 2, 2, 2, 2, 2, 2, 2, 3 ),
 ( 0.000000000000000000, 0.5000000000000000000, 1.000000000000000000 ),
 ( 0.000000000000000000, 0.01041666666666666609, 0.02083333333333333218, 0.03125000000000000000, 0.04166666666666666435, 0.05208333333333333565, 0.06250000000000000000, 0.07291666666666667129, 0.08333333333333332871, 0.09375000000000000000, 0.1041666666666666713, 0.1145833333333333287, 0.1250000000000000000, 0.1354166666666666574, 0.1458333333333333426, 0.1562500000000000000, 0.1666666666666666574, 0.1770833333333333426, 0.1875000000000000000, 0.1979166666666666574, 0.2083333333333333426, 0.2187500000000000000, 0.2291666666666666574, 0.2395833333333333426, 0.2500000000000000000, 0.2604166666666666852, 0.2708333333333333148, 0.2812500000000000000, 0.2916666666666666852, 0.3020833333333333148, 0.3125000000000000000, 0.3229166666666666852, 0.3333333333333333148, 0.3437500000000000000, 0.3541666666666666852, 0.3645833333333333148, 0.3750000000000000000, 0.3854166666666666852, 0.3958333333333333148, 0.4062500000000000000, 0.4166666666666666852, 0.4270833333333333148, 0.4375000000000000000, 0.4479166666666666852, 0.4583333333333333148, 0.4687500000000000000, 0.4791666666666666852, 0.4895833333333333148, 0.5000000000000000000, 0.5104166666666666297, 0.5208333333333333703, 0.5312500000000000000, 0.5416666666666666297, 0.5520833333333333703, 0.5625000000000000000, 0.5729166666666666297, 0.5833333333333333703, 0.5937500000000000000, 0.6041666666666666297, 0.6145833333333333703, 0.6250000000000000000, 0.6354166666666666297, 0.6458333333333333703, 0.6562500000000000000, 0.6666666666666666297, 0.6770833333333333703, 0.6875000000000000000, 0.6979166666666666297, 0.7083333333333333703, 0.7187500000000000000, 0.7291666666666666297, 0.7395833333333333703, 0.7500000000000000000, 0.7604166666666666297, 0.7708333333333333703, 0.7812500000000000000, 0.7916666666666666297, 0.8020833333333333703, 0.8125000000000000000, 0.8229166666666666297, 0.8333333333333333703, 0.8437500000000000000, 0.8541666666666666297, 0.8645833333333333703, 0.8750000000000000000, 0.8854166666666666297, 0.8958333333333333703, 0.9062500000000000000, 0.9166666666666666297, 0.9270833333333333703, 0.9375000000000000000, 0.9479166666666666297, 0.9583333333333333703, 0.9687500000000000000, 0.9791666666666666297, 0.9895833333333333703, 1.000000000000000000 ),
 .UNSPECIFIED. ) 
 GEOMETRIC_REPRESENTATION_ITEM ( )  RATIONAL_B_SPLINE_SURFACE ( (
 ( 1.000000000000000000, 0.9659258262890683122, 1.000000000000000000, 0.9659258262890683122, 1.000000000000000000, 0.9659258262890683122, 1.000000000000000000, 0.9659258262890683122, 1.000000000000000000, 0.9659258262890683122, 1.000000000000000000, 0.9659258262890683122, 1.000000000000000000, 0.9659258262890683122, 1.000000000000000000, 0.9659258262890683122, 1.000000000000000000, 0.9659258262890683122, 1.000000000000000000, 0.9659258262890683122, 1.000000000000000000, 0.9659258262890683122, 1.000000000000000000, 0.9659258262890683122, 1.000000000000000000, 0.9659258262890683122, 1.000000000000000000, 0.9659258262890683122, 1.000000000000000000, 0.9659258262890683122, 1.000000000000000000, 0.9659258262890683122, 1.000000000000000000, 0.9659258262890683122, 1.000000000000000000, 0.9659258262890683122, 1.000000000000000000, 0.9659258262890683122, 1.000000000000000000, 0.9659258262890683122, 1.000000000000000000, 0.9659258262890683122, 1.000000000000000000, 0.9659258262890683122, 1.000000000000000000, 0.9659258262890683122, 1.000000000000000000, 0.9659258262890683122, 1.000000000000000000, 0.9659258262890683122, 1.000000000000000000, 0.9659258262890683122, 1.000000000000000000, 0.9659258262890683122, 1.000000000000000000, 0.9659258262890683122, 1.000000000000000000, 0.9659258262890683122, 1.000000000000000000, 0.9659258262890683122, 1.000000000000000000, 0.9659258262890683122, 1.000000000000000000, 0.9659258262890683122, 1.000000000000000000, 0.9659258262890683122, 1.000000000000000000, 0.9659258262890683122, 1.000000000000000000, 0.9659258262890683122, 1.000000000000000000, 0.9659258262890683122, 1.000000000000000000, 0.9659258262890683122, 1.000000000000000000, 0.9659258262890683122, 1.000000000000000000, 0.9659258262890683122, 1.000000000000000000, 0.9659258262890683122, 1.000000000000000000, 0.9659258262890683122, 1.000000000000000000, 0.9659258262890683122, 1.000000000000000000, 0.9659258262890683122, 1.000000000000000000, 0.9659258262890683122, 1.000000000000000000, 0.9659258262890683122, 1.000000000000000000, 0.9659258262890683122, 1.000000000000000000, 0.9659258262890683122, 1.000000000000000000, 0.9659258262890683122, 1.000000000000000000, 0.9659258262890683122, 1.000000000000000000, 0.9659258262890683122, 1.000000000000000000, 0.9659258262890683122, 1.000000000000000000, 0.9659258262890683122, 1.000000000000000000, 0.9659258262890683122, 1.000000000000000000, 0.9659258262890683122, 1.000000000000000000, 0.9659258262890683122, 1.000000000000000000, 0.9659258262890683122, 1.000000000000000000, 0.9659258262890683122, 1.000000000000000000, 0.9659258262890683122, 1.000000000000000000, 0.9659258262890683122, 1.000000000000000000, 0.9659258262890683122, 1.000000000000000000, 0.9659258262890683122, 1.000000000000000000, 0.9659258262890683122, 1.000000000000000000, 0.9659258262890683122, 1.000000000000000000, 0.9659258262890683122, 1.000000000000000000, 0.9659258262890683122, 1.000000000000000000, 0.9659258262890683122, 1.000000000000000000, 0.9659258262890683122, 1.000000000000000000, 0.9659258262890683122, 1.000000000000000000, 0.9659258262890683122, 1.000000000000000000, 0.9659258262890683122, 1.000000000000000000, 0.9659258262890683122, 1.000000000000000000, 0.9659258262890683122, 1.000000000000000000, 0.9659258262890683122, 1.000000000000000000, 0.9659258262890683122, 1.000000000000000000, 0.9659258262890683122, 1.000000000000000000, 0.9659258262890683122, 1.000000000000000000, 0.9659258262890683122, 1.000000000000000000, 0.9659258262890683122, 1.000000000000000000, 0.9659258262890683122, 1.000000000000000000, 0.9659258262890683122, 1.000000000000000000, 0.9659258262890683122, 1.000000000000000000, 0.9659258262890683122, 1.000000000000000000, 0.9659258262890683122, 1.000000000000000000, 0.9659258262890683122, 1.000000000000000000, 0.9659258262890683122, 1.000000000000000000, 0.9659258262890683122, 1.000000000000000000, 0.9659258262890683122, 1.000000000000000000, 0.9659258262890683122, 1.000000000000000000, 0.9659258262890683122, 1.000000000000000000, 0.9659258262890683122, 1.000000000000000000, 0.9659258262890683122, 1.000000000000000000, 0.9659258262890683122, 1.000000000000000000, 0.9659258262890683122, 1.000000000000000000, 0.9659258262890683122, 1.000000000000000000, 0.9659258262890683122, 1.000000000000000000, 0.9659258262890683122, 1.000000000000000000),
 ( 0.3333333333333333703, 0.3219752754296894559, 0.3333333333333333703, 0.3219752754296894559, 0.3333333333333333703, 0.3219752754296894559, 0.3333333333333333703, 0.3219752754296894559, 0.3333333333333333703, 0.3219752754296894559, 0.3333333333333333703, 0.3219752754296894559, 0.3333333333333333703, 0.3219752754296894559, 0.3333333333333333703, 0.3219752754296894559, 0.3333333333333333703, 0.3219752754296894559, 0.3333333333333333703, 0.3219752754296894559, 0.3333333333333333703, 0.3219752754296894559, 0.3333333333333333703, 0.3219752754296894559, 0.3333333333333333703, 0.3219752754296894559, 0.3333333333333333703, 0.3219752754296894559, 0.3333333333333333703, 0.3219752754296894559, 0.3333333333333333703, 0.3219752754296894559, 0.3333333333333333703, 0.3219752754296894559, 0.3333333333333333703, 0.3219752754296894559, 0.3333333333333333703, 0.3219752754296894559, 0.3333333333333333703, 0.3219752754296894559, 0.3333333333333333703, 0.3219752754296894559, 0.3333333333333333703, 0.3219752754296894559, 0.3333333333333333703, 0.3219752754296894559, 0.3333333333333333703, 0.3219752754296894559, 0.3333333333333333703, 0.3219752754296894559, 0.3333333333333333703, 0.3219752754296894559, 0.3333333333333333703, 0.3219752754296894559, 0.3333333333333333703, 0.3219752754296894559, 0.3333333333333333703, 0.3219752754296894559, 0.3333333333333333703, 0.3219752754296894559, 0.3333333333333333703, 0.3219752754296894559, 0.3333333333333333703, 0.3219752754296894559, 0.3333333333333333703, 0.3219752754296894559, 0.3333333333333333703, 0.3219752754296894559, 0.3333333333333333703, 0.3219752754296894559, 0.3333333333333333703, 0.3219752754296894559, 0.3333333333333333703, 0.3219752754296894559, 0.3333333333333333703, 0.3219752754296894559, 0.3333333333333333703, 0.3219752754296894559, 0.3333333333333333703, 0.3219752754296894559, 0.3333333333333333703, 0.3219752754296894559, 0.3333333333333333703, 0.3219752754296894559, 0.3333333333333333703, 0.3219752754296894559, 0.3333333333333333703, 0.3219752754296894559, 0.3333333333333333703, 0.3219752754296894559, 0.3333333333333333703, 0.3219752754296894559, 0.3333333333333333703, 0.3219752754296894559, 0.3333333333333333703, 0.3219752754296894559, 0.3333333333333333703, 0.3219752754296894559, 0.3333333333333333703, 0.3219752754296894559, 0.3333333333333333703, 0.3219752754296894559, 0.3333333333333333703, 0.3219752754296894559, 0.3333333333333333703, 0.3219752754296894559, 0.3333333333333333703, 0.3219752754296894559, 0.3333333333333333703, 0.3219752754296894559, 0.3333333333333333703, 0.3219752754296894559, 0.3333333333333333703, 0.3219752754296894559, 0.3333333333333333703, 0.3219752754296894559, 0.3333333333333333703, 0.3219752754296894559, 0.3333333333333333703, 0.3219752754296894559, 0.3333333333333333703, 0.3219752754296894559, 0.3333333333333333703, 0.3219752754296894559, 0.3333333333333333703, 0.3219752754296894559, 0.3333333333333333703, 0.3219752754296894559, 0.3333333333333333703, 0.3219752754296894559, 0.3333333333333333703, 0.3219752754296894559, 0.3333333333333333703, 0.3219752754296894559, 0.3333333333333333703, 0.3219752754296894559, 0.3333333333333333703, 0.3219752754296894559, 0.3333333333333333703, 0.3219752754296894559, 0.3333333333333333703, 0.3219752754296894559, 0.3333333333333333703, 0.3219752754296894559, 0.3333333333333333703, 0.3219752754296894559, 0.3333333333333333703, 0.3219752754296894559, 0.3333333333333333703, 0.3219752754296894559, 0.3333333333333333703, 0.3219752754296894559, 0.3333333333333333703, 0.3219752754296894559, 0.3333333333333333703, 0.3219752754296894559, 0.3333333333333333703, 0.3219752754296894559, 0.3333333333333333703, 0.3219752754296894559, 0.3333333333333333703, 0.3219752754296894559, 0.3333333333333333703, 0.3219752754296894559, 0.3333333333333333703, 0.3219752754296894559, 0.3333333333333333703, 0.3219752754296894559, 0.3333333333333333703, 0.3219752754296894559, 0.3333333333333333703, 0.3219752754296894559, 0.3333333333333333703, 0.3219752754296894559, 0.3333333333333333703, 0.3219752754296894559, 0.3333333333333333703, 0.3219752754296894559, 0.3333333333333333703, 0.3219752754296894559, 0.3333333333333333703, 0.3219752754296894559, 0.3333333333333333703, 0.3219752754296894559, 0.3333333333333333703, 0.3219752754296894559, 0.3333333333333333703, 0.3219752754296894559, 0.3333333333333333703, 0.3219752754296894559, 0.3333333333333333703, 0.3219752754296894559, 0.3333333333333333703),
 ( 0.3333333333333333703, 0.3219752754296894559, 0.3333333333333333703, 0.3219752754296894559, 0.3333333333333333703, 0.3219752754296894559, 0.3333333333333333703, 0.3219752754296894559, 0.3333333333333333703, 0.3219752754296894559, 0.3333333333333333703, 0.3219752754296894559, 0.3333333333333333703, 0.3219752754296894559, 0.3333333333333333703, 0.3219752754296894559, 0.3333333333333333703, 0.3219752754296894559, 0.3333333333333333703, 0.3219752754296894559, 0.3333333333333333703, 0.3219752754296894559, 0.3333333333333333703, 0.3219752754296894559, 0.3333333333333333703, 0.3219752754296894559, 0.3333333333333333703, 0.3219752754296894559, 0.3333333333333333703, 0.3219752754296894559, 0.3333333333333333703, 0.3219752754296894559, 0.3333333333333333703, 0.3219752754296894559, 0.3333333333333333703, 0.3219752754296894559, 0.3333333333333333703, 0.3219752754296894559, 0.3333333333333333703, 0.3219752754296894559, 0.3333333333333333703, 0.3219752754296894559, 0.3333333333333333703, 0.3219752754296894559, 0.3333333333333333703, 0.3219752754296894559, 0.3333333333333333703, 0.3219752754296894559, 0.3333333333333333703, 0.3219752754296894559, 0.3333333333333333703, 0.3219752754296894559, 0.3333333333333333703, 0.3219752754296894559, 0.3333333333333333703, 0.3219752754296894559, 0.3333333333333333703, 0.3219752754296894559, 0.3333333333333333703, 0.3219752754296894559, 0.3333333333333333703, 0.3219752754296894559, 0.3333333333333333703, 0.3219752754296894559, 0.3333333333333333703, 0.3219752754296894559, 0.3333333333333333703, 0.3219752754296894559, 0.3333333333333333703, 0.3219752754296894559, 0.3333333333333333703, 0.3219752754296894559, 0.3333333333333333703, 0.3219752754296894559, 0.3333333333333333703, 0.3219752754296894559, 0.3333333333333333703, 0.3219752754296894559, 0.3333333333333333703, 0.3219752754296894559, 0.3333333333333333703, 0.3219752754296894559, 0.3333333333333333703, 0.3219752754296894559, 0.3333333333333333703, 0.3219752754296894559, 0.3333333333333333703, 0.3219752754296894559, 0.3333333333333333703, 0.3219752754296894559, 0.3333333333333333703, 0.3219752754296894559, 0.3333333333333333703, 0.3219752754296894559, 0.3333333333333333703, 0.3219752754296894559, 0.3333333333333333703, 0.3219752754296894559, 0.3333333333333333703, 0.3219752754296894559, 0.3333333333333333703, 0.3219752754296894559, 0.3333333333333333703, 0.3219752754296894559, 0.3333333333333333703, 0.3219752754296894559, 0.3333333333333333703, 0.3219752754296894559, 0.3333333333333333703, 0.3219752754296894559, 0.3333333333333333703, 0.3219752754296894559, 0.3333333333333333703, 0.3219752754296894559, 0.3333333333333333703, 0.3219752754296894559, 0.3333333333333333703, 0.3219752754296894559, 0.3333333333333333703, 0.3219752754296894559, 0.3333333333333333703, 0.3219752754296894559, 0.3333333333333333703, 0.3219752754296894559, 0.3333333333333333703, 0.3219752754296894559, 0.3333333333333333703, 0.3219752754296894559, 0.3333333333333333703, 0.3219752754296894559, 0.3333333333333333703, 0.3219752754296894559, 0.3333333333333333703, 0.3219752754296894559, 0.3333333333333333703, 0.3219752754296894559, 0.3333333333333333703, 0.3219752754296894559, 0.3333333333333333703, 0.3219752754296894559, 0.3333333333333333703, 0.3219752754296894559, 0.3333333333333333703, 0.3219752754296894559, 0.3333333333333333703, 0.3219752754296894559, 0.3333333333333333703, 0.3219752754296894559, 0.3333333333333333703, 0.3219752754296894559, 0.3333333333333333703, 0.3219752754296894559, 0.3333333333333333703, 0.3219752754296894559, 0.3333333333333333703, 0.3219752754296894559, 0.3333333333333333703, 0.3219752754296894559, 0.3333333333333333703, 0.3219752754296894559, 0.3333333333333333703, 0.3219752754296894559, 0.3333333333333333703, 0.3219752754296894559, 0.3333333333333333703, 0.3219752754296894559, 0.3333333333333333703, 0.3219752754296894559, 0.3333333333333333703, 0.3219752754296894559, 0.3333333333333333703, 0.3219752754296894559, 0.3333333333333333703, 0.3219752754296894559, 0.3333333333333333703, 0.3219752754296894559, 0.3333333333333333703, 0.3219752754296894559, 0.3333333333333333703, 0.3219752754296894559, 0.3333333333333333703, 0.3219752754296894559, 0.3333333333333333703, 0.3219752754296894559, 0.3333333333333333703, 0.3219752754296894559, 0.3333333333333333703, 0.3219752754296894559, 0.3333333333333333703, 0.3219752754296894559, 0.3333333333333333703, 0.3219752754296894559, 0.3333333333333333703),
 ( 1.000000000000000000, 0.9659258262890683122, 1.000000000000000000, 0.9659258262890683122, 1.000000000000000000, 0.9659258262890683122, 1.000000000000000000, 0.9659258262890683122, 1.000000000000000000, 0.9659258262890683122, 1.000000000000000000, 0.9659258262890683122, 1.000000000000000000, 0.9659258262890683122, 1.000000000000000000, 0.9659258262890683122, 1.000000000000000000, 0.9659258262890683122, 1.000000000000000000, 0.9659258262890683122, 1.000000000000000000, 0.9659258262890683122, 1.000000000000000000, 0.9659258262890683122, 1.000000000000000000, 0.9659258262890683122, 1.000000000000000000, 0.9659258262890683122, 1.000000000000000000, 0.9659258262890683122, 1.000000000000000000, 0.9659258262890683122, 1.000000000000000000, 0.9659258262890683122, 1.000000000000000000, 0.9659258262890683122, 1.000000000000000000, 0.9659258262890683122, 1.000000000000000000, 0.9659258262890683122, 1.000000000000000000, 0.9659258262890683122, 1.000000000000000000, 0.9659258262890683122, 1.000000000000000000, 0.9659258262890683122, 1.000000000000000000, 0.9659258262890683122, 1.000000000000000000, 0.9659258262890683122, 1.000000000000000000, 0.9659258262890683122, 1.000000000000000000, 0.9659258262890683122, 1.000000000000000000, 0.9659258262890683122, 1.000000000000000000, 0.9659258262890683122, 1.000000000000000000, 0.9659258262890683122, 1.000000000000000000, 0.9659258262890683122, 1.000000000000000000, 0.9659258262890683122, 1.000000000000000000, 0.9659258262890683122, 1.000000000000000000, 0.9659258262890683122, 1.000000000000000000, 0.9659258262890683122, 1.000000000000000000, 0.9659258262890683122, 1.000000000000000000, 0.9659258262890683122, 1.000000000000000000, 0.9659258262890683122, 1.000000000000000000, 0.9659258262890683122, 1.000000000000000000, 0.9659258262890683122, 1.000000000000000000, 0.9659258262890683122, 1.000000000000000000, 0.9659258262890683122, 1.000000000000000000, 0.9659258262890683122, 1.000000000000000000, 0.9659258262890683122, 1.000000000000000000, 0.9659258262890683122, 1.000000000000000000, 0.9659258262890683122, 1.000000000000000000, 0.9659258262890683122, 1.000000000000000000, 0.9659258262890683122, 1.000000000000000000, 0.9659258262890683122, 1.000000000000000000, 0.9659258262890683122, 1.000000000000000000, 0.9659258262890683122, 1.000000000000000000, 0.9659258262890683122, 1.000000000000000000, 0.9659258262890683122, 1.000000000000000000, 0.9659258262890683122, 1.000000000000000000, 0.9659258262890683122, 1.000000000000000000, 0.9659258262890683122, 1.000000000000000000, 0.9659258262890683122, 1.000000000000000000, 0.9659258262890683122, 1.000000000000000000, 0.9659258262890683122, 1.000000000000000000, 0.9659258262890683122, 1.000000000000000000, 0.9659258262890683122, 1.000000000000000000, 0.9659258262890683122, 1.000000000000000000, 0.9659258262890683122, 1.000000000000000000, 0.9659258262890683122, 1.000000000000000000, 0.9659258262890683122, 1.000000000000000000, 0.9659258262890683122, 1.000000000000000000, 0.9659258262890683122, 1.000000000000000000, 0.9659258262890683122, 1.000000000000000000, 0.9659258262890683122, 1.000000000000000000, 0.9659258262890683122, 1.000000000000000000, 0.9659258262890683122, 1.000000000000000000, 0.9659258262890683122, 1.000000000000000000, 0.9659258262890683122, 1.000000000000000000, 0.9659258262890683122, 1.000000000000000000, 0.9659258262890683122, 1.000000000000000000, 0.9659258262890683122, 1.000000000000000000, 0.9659258262890683122, 1.000000000000000000, 0.9659258262890683122, 1.000000000000000000, 0.9659258262890683122, 1.000000000000000000, 0.9659258262890683122, 1.000000000000000000, 0.9659258262890683122, 1.000000000000000000, 0.9659258262890683122, 1.000000000000000000, 0.9659258262890683122, 1.000000000000000000, 0.9659258262890683122, 1.000000000000000000, 0.9659258262890683122, 1.000000000000000000, 0.9659258262890683122, 1.000000000000000000, 0.9659258262890683122, 1.000000000000000000, 0.9659258262890683122, 1.000000000000000000, 0.9659258262890683122, 1.000000000000000000, 0.9659258262890683122, 1.000000000000000000, 0.9659258262890683122, 1.000000000000000000, 0.9659258262890683122, 1.000000000000000000, 0.9659258262890683122, 1.000000000000000000, 0.9659258262890683122, 1.000000000000000000, 0.9659258262890683122, 1.000000000000000000, 0.9659258262890683122, 1.000000000000000000),
 ( 0.3333333333333333703, 0.3219752754296894559, 0.3333333333333333703, 0.3219752754296894559, 0.3333333333333333703, 0.3219752754296894559, 0.3333333333333333703, 0.3219752754296894559, 0.3333333333333333703, 0.3219752754296894559, 0.3333333333333333703, 0.3219752754296894559, 0.3333333333333333703, 0.3219752754296894559, 0.3333333333333333703, 0.3219752754296894559, 0.3333333333333333703, 0.3219752754296894559, 0.3333333333333333703, 0.3219752754296894559, 0.3333333333333333703, 0.3219752754296894559, 0.3333333333333333703, 0.3219752754296894559, 0.3333333333333333703, 0.3219752754296894559, 0.3333333333333333703, 0.3219752754296894559, 0.3333333333333333703, 0.3219752754296894559, 0.3333333333333333703, 0.3219752754296894559, 0.3333333333333333703, 0.3219752754296894559, 0.3333333333333333703, 0.3219752754296894559, 0.3333333333333333703, 0.3219752754296894559, 0.3333333333333333703, 0.3219752754296894559, 0.3333333333333333703, 0.3219752754296894559, 0.3333333333333333703, 0.3219752754296894559, 0.3333333333333333703, 0.3219752754296894559, 0.3333333333333333703, 0.3219752754296894559, 0.3333333333333333703, 0.3219752754296894559, 0.3333333333333333703, 0.3219752754296894559, 0.3333333333333333703, 0.3219752754296894559, 0.3333333333333333703, 0.3219752754296894559, 0.3333333333333333703, 0.3219752754296894559, 0.3333333333333333703, 0.3219752754296894559, 0.3333333333333333703, 0.3219752754296894559, 0.3333333333333333703, 0.3219752754296894559, 0.3333333333333333703, 0.3219752754296894559, 0.3333333333333333703, 0.3219752754296894559, 0.3333333333333333703, 0.3219752754296894559, 0.3333333333333333703, 0.3219752754296894559, 0.3333333333333333703, 0.3219752754296894559, 0.3333333333333333703, 0.3219752754296894559, 0.3333333333333333703, 0.3219752754296894559, 0.3333333333333333703, 0.3219752754296894559, 0.3333333333333333703, 0.3219752754296894559, 0.3333333333333333703, 0.3219752754296894559, 0.3333333333333333703, 0.3219752754296894559, 0.3333333333333333703, 0.3219752754296894559, 0.3333333333333333703, 0.3219752754296894559, 0.3333333333333333703, 0.3219752754296894559, 0.3333333333333333703, 0.3219752754296894559, 0.3333333333333333703, 0.3219752754296894559, 0.3333333333333333703, 0.3219752754296894559, 0.3333333333333333703, 0.3219752754296894559, 0.3333333333333333703, 0.3219752754296894559, 0.3333333333333333703, 0.3219752754296894559, 0.3333333333333333703, 0.3219752754296894559, 0.3333333333333333703, 0.3219752754296894559, 0.3333333333333333703, 0.3219752754296894559, 0.3333333333333333703, 0.3219752754296894559, 0.3333333333333333703, 0.3219752754296894559, 0.3333333333333333703, 0.3219752754296894559, 0.3333333333333333703, 0.3219752754296894559, 0.3333333333333333703, 0.3219752754296894559, 0.3333333333333333703, 0.3219752754296894559, 0.3333333333333333703, 0.3219752754296894559, 0.3333333333333333703, 0.3219752754296894559, 0.3333333333333333703, 0.3219752754296894559, 0.3333333333333333703, 0.3219752754296894559, 0.3333333333333333703, 0.3219752754296894559, 0.3333333333333333703, 0.3219752754296894559, 0.3333333333333333703, 0.3219752754296894559, 0.3333333333333333703, 0.3219752754296894559, 0.3333333333333333703, 0.3219752754296894559, 0.3333333333333333703, 0.3219752754296894559, 0.3333333333333333703, 0.3219752754296894559, 0.3333333333333333703, 0.3219752754296894559, 0.3333333333333333703, 0.3219752754296894559, 0.3333333333333333703, 0.3219752754296894559, 0.3333333333333333703, 0.3219752754296894559, 0.3333333333333333703, 0.3219752754296894559, 0.3333333333333333703, 0.3219752754296894559, 0.3333333333333333703, 0.3219752754296894559, 0.3333333333333333703, 0.3219752754296894559, 0.3333333333333333703, 0.3219752754296894559, 0.3333333333333333703, 0.3219752754296894559, 0.3333333333333333703, 0.3219752754296894559, 0.3333333333333333703, 0.3219752754296894559, 0.3333333333333333703, 0.3219752754296894559, 0.3333333333333333703, 0.3219752754296894559, 0.3333333333333333703, 0.3219752754296894559, 0.3333333333333333703, 0.3219752754296894559, 0.3333333333333333703, 0.3219752754296894559, 0.3333333333333333703, 0.3219752754296894559, 0.3333333333333333703, 0.3219752754296894559, 0.3333333333333333703, 0.3219752754296894559, 0.3333333333333333703, 0.3219752754296894559, 0.3333333333333333703, 0.3219752754296894559, 0.3333333333333333703, 0.3219752754296894559, 0.3333333333333333703, 0.3219752754296894559, 0.3333333333333333703),
 ( 0.3333333333333333703, 0.3219752754296894559, 0.3333333333333333703, 0.3219752754296894559, 0.3333333333333333703, 0.3219752754296894559, 0.3333333333333333703, 0.3219752754296894559, 0.3333333333333333703, 0.3219752754296894559, 0.3333333333333333703, 0.3219752754296894559, 0.3333333333333333703, 0.3219752754296894559, 0.3333333333333333703, 0.3219752754296894559, 0.3333333333333333703, 0.3219752754296894559, 0.3333333333333333703, 0.3219752754296894559, 0.3333333333333333703, 0.3219752754296894559, 0.3333333333333333703, 0.3219752754296894559, 0.3333333333333333703, 0.3219752754296894559, 0.3333333333333333703, 0.3219752754296894559, 0.3333333333333333703, 0.3219752754296894559, 0.3333333333333333703, 0.3219752754296894559, 0.3333333333333333703, 0.3219752754296894559, 0.3333333333333333703, 0.3219752754296894559, 0.3333333333333333703, 0.3219752754296894559, 0.3333333333333333703, 0.3219752754296894559, 0.3333333333333333703, 0.3219752754296894559, 0.3333333333333333703, 0.3219752754296894559, 0.3333333333333333703, 0.3219752754296894559, 0.3333333333333333703, 0.3219752754296894559, 0.3333333333333333703, 0.3219752754296894559, 0.3333333333333333703, 0.3219752754296894559, 0.3333333333333333703, 0.3219752754296894559, 0.3333333333333333703, 0.3219752754296894559, 0.3333333333333333703, 0.3219752754296894559, 0.3333333333333333703, 0.3219752754296894559, 0.3333333333333333703, 0.3219752754296894559, 0.3333333333333333703, 0.3219752754296894559, 0.3333333333333333703, 0.3219752754296894559, 0.3333333333333333703, 0.3219752754296894559, 0.3333333333333333703, 0.3219752754296894559, 0.3333333333333333703, 0.3219752754296894559, 0.3333333333333333703, 0.3219752754296894559, 0.3333333333333333703, 0.3219752754296894559, 0.3333333333333333703, 0.3219752754296894559, 0.3333333333333333703, 0.3219752754296894559, 0.3333333333333333703, 0.3219752754296894559, 0.3333333333333333703, 0.3219752754296894559, 0.3333333333333333703, 0.3219752754296894559, 0.3333333333333333703, 0.3219752754296894559, 0.3333333333333333703, 0.3219752754296894559, 0.3333333333333333703, 0.3219752754296894559, 0.3333333333333333703, 0.3219752754296894559, 0.3333333333333333703, 0.3219752754296894559, 0.3333333333333333703, 0.3219752754296894559, 0.3333333333333333703, 0.3219752754296894559, 0.3333333333333333703, 0.3219752754296894559, 0.3333333333333333703, 0.3219752754296894559, 0.3333333333333333703, 0.3219752754296894559, 0.3333333333333333703, 0.3219752754296894559, 0.3333333333333333703, 0.3219752754296894559, 0.3333333333333333703, 0.3219752754296894559, 0.3333333333333333703, 0.3219752754296894559, 0.3333333333333333703, 0.3219752754296894559, 0.3333333333333333703, 0.3219752754296894559, 0.3333333333333333703, 0.3219752754296894559, 0.3333333333333333703, 0.3219752754296894559, 0.3333333333333333703, 0.3219752754296894559, 0.3333333333333333703, 0.3219752754296894559, 0.3333333333333333703, 0.3219752754296894559, 0.3333333333333333703, 0.3219752754296894559, 0.3333333333333333703, 0.3219752754296894559, 0.3333333333333333703, 0.3219752754296894559, 0.3333333333333333703, 0.3219752754296894559, 0.3333333333333333703, 0.3219752754296894559, 0.3333333333333333703, 0.3219752754296894559, 0.3333333333333333703, 0.3219752754296894559, 0.3333333333333333703, 0.3219752754296894559, 0.3333333333333333703, 0.3219752754296894559, 0.3333333333333333703, 0.3219752754296894559, 0.3333333333333333703, 0.3219752754296894559, 0.3333333333333333703, 0.3219752754296894559, 0.3333333333333333703, 0.3219752754296894559, 0.3333333333333333703, 0.3219752754296894559, 0.3333333333333333703, 0.3219752754296894559, 0.3333333333333333703, 0.3219752754296894559, 0.3333333333333333703, 0.3219752754296894559, 0.3333333333333333703, 0.3219752754296894559, 0.3333333333333333703, 0.3219752754296894559, 0.3333333333333333703, 0.3219752754296894559, 0.3333333333333333703, 0.3219752754296894559, 0.3333333333333333703, 0.3219752754296894559, 0.3333333333333333703, 0.3219752754296894559, 0.3333333333333333703, 0.3219752754296894559, 0.3333333333333333703, 0.3219752754296894559, 0.3333333333333333703, 0.3219752754296894559, 0.3333333333333333703, 0.3219752754296894559, 0.3333333333333333703, 0.3219752754296894559, 0.3333333333333333703, 0.3219752754296894559, 0.3333333333333333703, 0.3219752754296894559, 0.3333333333333333703, 0.3219752754296894559, 0.3333333333333333703, 0.3219752754296894559, 0.3333333333333333703),
 ( 1.000000000000000000, 0.9659258262890683122, 1.000000000000000000, 0.9659258262890683122, 1.000000000000000000, 0.9659258262890683122, 1.000000000000000000, 0.9659258262890683122, 1.000000000000000000, 0.9659258262890683122, 1.000000000000000000, 0.9659258262890683122, 1.000000000000000000, 0.9659258262890683122, 1.000000000000000000, 0.9659258262890683122, 1.000000000000000000, 0.9659258262890683122, 1.000000000000000000, 0.9659258262890683122, 1.000000000000000000, 0.9659258262890683122, 1.000000000000000000, 0.9659258262890683122, 1.000000000000000000, 0.9659258262890683122, 1.000000000000000000, 0.9659258262890683122, 1.000000000000000000, 0.9659258262890683122, 1.000000000000000000, 0.9659258262890683122, 1.000000000000000000, 0.9659258262890683122, 1.000000000000000000, 0.9659258262890683122, 1.000000000000000000, 0.9659258262890683122, 1.000000000000000000, 0.9659258262890683122, 1.000000000000000000, 0.9659258262890683122, 1.000000000000000000, 0.9659258262890683122, 1.000000000000000000, 0.9659258262890683122, 1.000000000000000000, 0.9659258262890683122, 1.000000000000000000, 0.9659258262890683122, 1.000000000000000000, 0.9659258262890683122, 1.000000000000000000, 0.9659258262890683122, 1.000000000000000000, 0.9659258262890683122, 1.000000000000000000, 0.9659258262890683122, 1.000000000000000000, 0.9659258262890683122, 1.000000000000000000, 0.9659258262890683122, 1.000000000000000000, 0.9659258262890683122, 1.000000000000000000, 0.9659258262890683122, 1.000000000000000000, 0.9659258262890683122, 1.000000000000000000, 0.9659258262890683122, 1.000000000000000000, 0.9659258262890683122, 1.000000000000000000, 0.9659258262890683122, 1.000000000000000000, 0.9659258262890683122, 1.000000000000000000, 0.9659258262890683122, 1.000000000000000000, 0.9659258262890683122, 1.000000000000000000, 0.9659258262890683122, 1.000000000000000000, 0.9659258262890683122, 1.000000000000000000, 0.9659258262890683122, 1.000000000000000000, 0.9659258262890683122, 1.000000000000000000, 0.9659258262890683122, 1.000000000000000000, 0.9659258262890683122, 1.000000000000000000, 0.9659258262890683122, 1.000000000000000000, 0.9659258262890683122, 1.000000000000000000, 0.9659258262890683122, 1.000000000000000000, 0.9659258262890683122, 1.000000000000000000, 0.9659258262890683122, 1.000000000000000000, 0.9659258262890683122, 1.000000000000000000, 0.9659258262890683122, 1.000000000000000000, 0.9659258262890683122, 1.000000000000000000, 0.9659258262890683122, 1.000000000000000000, 0.9659258262890683122, 1.000000000000000000, 0.9659258262890683122, 1.000000000000000000, 0.9659258262890683122, 1.000000000000000000, 0.9659258262890683122, 1.000000000000000000, 0.9659258262890683122, 1.000000000000000000, 0.9659258262890683122, 1.000000000000000000, 0.9659258262890683122, 1.000000000000000000, 0.9659258262890683122, 1.000000000000000000, 0.9659258262890683122, 1.000000000000000000, 0.9659258262890683122, 1.000000000000000000, 0.9659258262890683122, 1.000000000000000000, 0.9659258262890683122, 1.000000000000000000, 0.9659258262890683122, 1.000000000000000000, 0.9659258262890683122, 1.000000000000000000, 0.9659258262890683122, 1.000000000000000000, 0.9659258262890683122, 1.000000000000000000, 0.9659258262890683122, 1.000000000000000000, 0.9659258262890683122, 1.000000000000000000, 0.9659258262890683122, 1.000000000000000000, 0.9659258262890683122, 1.000000000000000000, 0.9659258262890683122, 1.000000000000000000, 0.9659258262890683122, 1.000000000000000000, 0.9659258262890683122, 1.000000000000000000, 0.9659258262890683122, 1.000000000000000000, 0.9659258262890683122, 1.000000000000000000, 0.9659258262890683122, 1.000000000000000000, 0.9659258262890683122, 1.000000000000000000, 0.9659258262890683122, 1.000000000000000000, 0.9659258262890683122, 1.000000000000000000, 0.9659258262890683122, 1.000000000000000000, 0.9659258262890683122, 1.000000000000000000, 0.9659258262890683122, 1.000000000000000000, 0.9659258262890683122, 1.000000000000000000, 0.9659258262890683122, 1.000000000000000000, 0.9659258262890683122, 1.000000000000000000, 0.9659258262890683122, 1.000000000000000000, 0.9659258262890683122, 1.000000000000000000, 0.9659258262890683122, 1.000000000000000000, 0.9659258262890683122, 1.000000000000000000, 0.9659258262890683122, 1.000000000000000000, 0.9659258262890683122, 1.000000000000000000) ) ) 
 REPRESENTATION_ITEM ( '' )  SURFACE ( )  );
#519 = CARTESIAN_POINT ( 'NONE',  ( -10.00000000000000000, -17.18313764714974923, -16.36466261444977377 ) ) ;
#520 = ORIENTED_EDGE ( 'NONE', *, *, #14321, .T. ) ;
#521 = CARTESIAN_POINT ( 'NONE',  ( 0.1249999999999895917, 33.84386001800125143, 52.64142135623733765 ) ) ;
#522 = ORIENTED_EDGE ( 'NONE', *, *, #3988, .F. ) ;
#523 = DIRECTION ( 'NONE',  ( -1.156482317317871478E-16, 1.000000000000000000, 0.000000000000000000 ) ) ;
#524 = CARTESIAN_POINT ( 'NONE',  ( 2.500000000000000000, 2.357898499370431722, -2.818925648462311528E-15 ) ) ;
#525 = LINE ( 'NONE', #11565, #11597 ) ;
#526 = EDGE_CURVE ( 'NONE', #18598, #13355, #19142, .T. ) ;
#527 = DIRECTION ( 'NONE',  ( -1.942890293094023946E-16, 0.7071067811865453523, 0.7071067811865496822 ) ) ;
#528 = EDGE_CURVE ( 'NONE', #3513, #14696, #14857, .T. ) ;
#529 = VECTOR ( 'NONE', #12275, 1000.000000000000000 ) ;
#530 = VECTOR ( 'NONE', #4637, 1000.000000000000000 ) ;
#531 = CARTESIAN_POINT ( 'NONE',  ( 1.767766952966369987, 65.76776695296638309, 46.49999999999999289 ) ) ;
#532 = DIRECTION ( 'NONE',  ( 0.000000000000000000, 0.000000000000000000, -1.000000000000000000 ) ) ;
#533 = CARTESIAN_POINT ( 'NONE',  ( 4.101219330881941794, 26.84264068711924267, 59.64264068711931088 ) ) ;
#534 = DIRECTION ( 'NONE',  ( 1.000000000000000000, -0.000000000000000000, -0.000000000000000000 ) ) ;
#535 = VERTEX_POINT ( 'NONE', #8772 ) ;
#536 = CARTESIAN_POINT ( 'NONE',  ( -19.99999999999999645, -23.83517299489738051, 18.70117750791695954 ) ) ;
#537 = CARTESIAN_POINT ( 'NONE',  ( -1.767766952966370209, 65.76776695296638309, 46.80000000218494449 ) ) ;
#538 = CARTESIAN_POINT ( 'NONE',  ( -13.82508104294702100, -18.95583473709188382, 22.20507249208304401 ) ) ;
#539 = DIRECTION ( 'NONE',  ( 0.000000000000000000, 0.000000000000000000, -1.000000000000000000 ) ) ;
#540 = CARTESIAN_POINT ( 'NONE',  ( -14.83517299489739649, -18.99999999999997868, 20.01367750791695954 ) ) ;
#541 = CYLINDRICAL_SURFACE ( 'NONE', #12959, 2.750000000000000000 ) ;
#542 = CARTESIAN_POINT ( 'NONE',  ( -16.50457296725820555, -28.95583473709189803, 17.60742750791695599 ) ) ;
#543 = DIRECTION ( 'NONE',  ( 0.000000000000000000, 0.000000000000000000, 1.000000000000000000 ) ) ;
#544 = CARTESIAN_POINT ( 'NONE',  ( -13.82508104294702100, -18.95583473709188382, 27.45507249208304046 ) ) ;
#545 = EDGE_CURVE ( 'NONE', #16762, #576, #17802, .T. ) ;
#546 = CARTESIAN_POINT ( 'NONE',  ( 1.461580736456473684, 65.46158073645646880, 47.85000000109246798 ) ) ;
#547 = DIRECTION ( 'NONE',  ( 0.000000000000000000, 0.000000000000000000, -1.000000000000000000 ) ) ;
#548 = DIRECTION ( 'NONE',  ( -1.000000000000000000, 0.000000000000000000, 0.000000000000000000 ) ) ;
#549 = SURFACE_STYLE_FILL_AREA ( #12311 ) ;
#550 = CARTESIAN_POINT ( 'NONE',  ( -1.265664690411616068E-16, 66.06698730000000808, 47.15000000109247225 ) ) ;
#551 = LINE ( 'NONE', #3304, #5191 ) ;
#552 = ORIENTED_EDGE ( 'NONE', *, *, #4349, .F. ) ;
#553 = ORIENTED_EDGE ( 'NONE', *, *, #12530, .T. ) ;
#554 = CARTESIAN_POINT ( 'NONE',  ( -18.64274437364860049, -18.02023567606023491, 26.79882249208304401 ) ) ;
#555 = CARTESIAN_POINT ( 'NONE',  ( -19.41254052147350961, -21.64274437364857562, 15.86132249208304223 ) ) ;
#556 = ORIENTED_EDGE ( 'NONE', *, *, #4978, .F. ) ;
#557 = CARTESIAN_POINT ( 'NONE',  ( -18.04416526290808420, -24.63902057219074493, 28.98242750791696309 ) ) ;
#558 = DIRECTION ( 'NONE',  ( -1.000000000000000000, 0.000000000000000000, -0.000000000000000000 ) ) ;
#559 = CARTESIAN_POINT ( 'NONE',  ( -21.99999999999999289, -24.16482700510262305, 20.67382249208304046 ) ) ;
#560 = CARTESIAN_POINT ( 'NONE',  ( 2.066987300000002303, 63.14382582708705627, 47.50000000109246656 ) ) ;
#561 = EDGE_LOOP ( 'NONE', ( #1541, #12212 ) ) ;
#562 = ADVANCED_FACE ( 'NONE', ( #8873 ), #154, .T. ) ;
#563 = ORIENTED_EDGE ( 'NONE', *, *, #6960, .T. ) ;
#564 = LINE ( 'NONE', #18228, #7201 ) ;
#565 = FACE_OUTER_BOUND ( 'NONE', #15076, .T. ) ;
#566 = CARTESIAN_POINT ( 'NONE',  ( -2.066987300000001415, 64.85617417291294373, 47.90000000109247225 ) ) ;
#567 = DIRECTION ( 'NONE',  ( 0.000000000000000000, 1.000000000000000000, 0.000000000000000000 ) ) ;
#568 = LINE ( 'NONE', #6369, #960 ) ;
#569 = EDGE_CURVE ( 'NONE', #5562, #14997, #2796, .T. ) ;
#570 = FACE_OUTER_BOUND ( 'NONE', #5222, .T. ) ;
#571 = ADVANCED_BREP_SHAPE_REPRESENTATION ( '', ( #16938, #1791 ), #5851 ) ;
#572 = DIRECTION ( 'NONE',  ( -1.541976423090495633E-16, 0.000000000000000000, 1.000000000000000000 ) ) ;
#573 = ORIENTED_EDGE ( 'NONE', *, *, #9984, .T. ) ;
#574 = VERTEX_POINT ( 'NONE', #10335 ) ;
#575 = CARTESIAN_POINT ( 'NONE',  ( -8.855408670957631401, -20.64274437364852943, 31.38867750791695599 ) ) ;
#576 = VERTEX_POINT ( 'NONE', #13377 ) ;
#578 = VERTEX_POINT ( 'NONE', #19174 ) ;
#577 = ORIENTED_EDGE ( 'NONE', *, *, #17798, .T. ) ;
#579 = CARTESIAN_POINT ( 'NONE',  ( -15.16482700510262482, -20.99999999999997513, 37.73632249208304756 ) ) ;
#580 = CARTESIAN_POINT ( 'NONE',  ( -9.754982604823348780, -18.99630608921234654, 20.66992750791695954 ) ) ;
#581 = VECTOR ( 'NONE', #2799, 1000.000000000000000 ) ;
#582 = DIRECTION ( 'NONE',  ( 2.220446049250312834E-16, 0.7071067811865455743, 0.7071067811865493491 ) ) ;
#583 = CARTESIAN_POINT ( 'NONE',  ( 0.8561741729129460632, 66.06698730000000808, 49.30000000109246372 ) ) ;
#584 = DIRECTION ( 'NONE',  ( -0.000000000000000000, 0.000000000000000000, -1.000000000000000000 ) ) ;
#585 = EDGE_LOOP ( 'NONE', ( #18934, #14409, #5001, #12417 ) ) ;
#586 = CARTESIAN_POINT ( 'NONE',  ( -14.36097942780923731, -27.04416526290806999, 27.66992750791696665 ) ) ;
#587 = VERTEX_POINT ( 'NONE', #5745 ) ;
#588 = CARTESIAN_POINT ( 'NONE',  ( -41.00000000000000711, 53.00000000000000711, -24.49999999999999645 ) ) ;
#589 = EDGE_LOOP ( 'NONE', ( #3897, #9508, #16057, #4812 ) ) ;
#590 = CARTESIAN_POINT ( 'NONE',  ( 44.99999999999998579, 0.000000000000000000, -54.99999999999998579 ) ) ;
#591 = CARTESIAN_POINT ( 'NONE',  ( 5.799999999999985612, 29.65425233947092920, 56.47747564417436195 ) ) ;
#592 = DIRECTION ( 'NONE',  ( -1.156482317317871478E-16, 1.000000000000000000, 0.000000000000000000 ) ) ;
#593 = FACE_BOUND ( 'NONE', #7659, .T. ) ;
#594 = CIRCLE ( 'NONE', #10600, 4.000000000000001776 ) ;
#595 = CARTESIAN_POINT ( 'NONE',  ( 0.8561741729129460632, 66.06698729999999387, 47.70000000109248361 ) ) ;
#596 = CONTEXT_DEPENDENT_SHAPE_REPRESENTATION ( #3061, #10515 ) ;
#597 = CARTESIAN_POINT ( 'NONE',  ( -2.066987300000000971, 63.14382582708704916, 48.20000000109247651 ) ) ;
#598 = CARTESIAN_POINT ( 'NONE',  ( 5.799999999999985612, 29.65425233947092920, 56.47747564417436195 ) ) ;
#599 = VECTOR ( 'NONE', #2972, 1000.000000000000000 ) ;
#600 = CARTESIAN_POINT ( 'NONE',  ( 44.99999999999998579, 3.000000000000000000, -53.39999999999999147 ) ) ;
#601 = DIRECTION ( 'NONE',  ( 0.000000000000000000, 0.000000000000000000, -1.000000000000000000 ) ) ;
#602 = ORIENTED_EDGE ( 'NONE', *, *, #4334, .F. ) ;
#603 = CARTESIAN_POINT ( 'NONE',  ( -19.99999999999999645, -23.83517299489738051, 23.95117750791695954 ) ) ;
#604 = CARTESIAN_POINT ( 'NONE',  ( -50.00000000000002132, 3.000000000000000000, -60.00000000000002132 ) ) ;
#605 = ORIENTED_EDGE ( 'NONE', *, *, #6639, .T. ) ;
#606 = CARTESIAN_POINT ( 'NONE',  ( -15.16482700510263371, -18.99999999999997868, 37.73632249208303335 ) ) ;
#607 = AXIS2_PLACEMENT_3D ( 'NONE', #1336, #7408, #13378 ) ;
#608 = CARTESIAN_POINT ( 'NONE',  ( -12.48433729119799196, -22.35725562635139596, 33.36132249208304756 ) ) ;
#609 = AXIS2_PLACEMENT_3D ( 'NONE', #15894, #14234, #2648 ) ;
#610 = FILL_AREA_STYLE ('',( #3268 ) ) ;
#611 = ORIENTED_EDGE ( 'NONE', *, *, #18614, .F. ) ;
#612 = VECTOR ( 'NONE', #474, 1000.000000000000000 ) ;
#613 = DIRECTION ( 'NONE',  ( 1.000000000000000000, 0.000000000000000000, 0.000000000000000000 ) ) ;
#614 = ORIENTED_EDGE ( 'NONE', *, *, #3279, .F. ) ;
#615 = DIRECTION ( 'NONE',  ( 0.000000000000000000, 0.000000000000000000, 1.000000000000000000 ) ) ;
#616 = EDGE_CURVE ( 'NONE', #16789, #4517, #9072, .T. ) ;
#617 = ADVANCED_FACE ( 'NONE', ( #14763 ), #16425, .T. ) ;
#618 = CARTESIAN_POINT ( 'NONE',  ( 1.767766952966370653, 62.23223304703363112, 46.29999999999999716 ) ) ;
#619 = FACE_BOUND ( 'NONE', #18932, .T. ) ;
#620 = EDGE_CURVE ( 'NONE', #15312, #12747, #7305, .T. ) ;
#621 = VECTOR ( 'NONE', #523, 1000.000000000000000 ) ;
#622 = LINE ( 'NONE', #15618, #18616 ) ;
#623 = CARTESIAN_POINT ( 'NONE',  ( -1.767766952966370209, 65.76776695296638309, 45.09999999999999432 ) ) ;
#625 = EDGE_CURVE ( 'NONE', #3704, #982, #6141, .T. ) ;
#624 = DIRECTION ( 'NONE',  ( -0.000000000000000000, 1.000000000000000000, -0.000000000000000000 ) ) ;
#626 = VECTOR ( 'NONE', #2257, 1000.000000000000000 ) ;
#627 = DIRECTION ( 'NONE',  ( 0.000000000000000000, 0.000000000000000000, 1.000000000000000000 ) ) ;
#628 = VERTEX_POINT ( 'NONE', #13272 ) ;
#629 = CARTESIAN_POINT ( 'NONE',  ( -14.83517299489739649, -18.99999999999997868, 35.76367750791695954 ) ) ;
#630 = AXIS2_PLACEMENT_3D ( 'NONE', #16972, #17154, #15490 ) ;
#631 = CARTESIAN_POINT ( 'NONE',  ( 1.767766952966369987, 65.76776695296638309, 46.60000000218494165 ) ) ;
#632 = EDGE_CURVE ( 'NONE', #7648, #3232, #16629, .T. ) ;
#633 = CARTESIAN_POINT ( 'NONE',  ( -9.955834737091903364, -25.17491895705294880, 23.51757249208304401 ) ) ;
#634 = VECTOR ( 'NONE', #11787, 1000.000000000000000 ) ;
#635 = LINE ( 'NONE', #15629, #18156 ) ;
#636 = CARTESIAN_POINT ( 'NONE',  ( -12.35725562635143682, -19.75228648362908501, 15.20117750791695777 ) ) ;
#637 = FACE_OUTER_BOUND ( 'NONE', #1554, .T. ) ;
#638 = CARTESIAN_POINT ( 'NONE',  ( -19.41254052147348830, -26.35725562635142083, 34.01367750791696665 ) ) ;
#639 = FACE_OUTER_BOUND ( 'NONE', #6765, .T. ) ;
#640 = CARTESIAN_POINT ( 'NONE',  ( -10.75228648362912232, -21.35725562635138530, 22.86132249208304401 ) ) ;
#641 = EDGE_CURVE ( 'NONE', #12504, #12460, #12102, .T. ) ;
#642 = CARTESIAN_POINT ( 'NONE',  ( -2.066987300000001859, 64.85617417291294373, 45.70000000109248361 ) ) ;
#643 = CARTESIAN_POINT ( 'NONE',  ( -24.00000000000000000, 113.0000000000000000, 30.00000000000000000 ) ) ;
#644 = CARTESIAN_POINT ( 'NONE',  ( 46.99999999999998579, 16.75735931288065572, 56.99999999999997158 ) ) ;
#645 = VECTOR ( 'NONE', #16601, 1000.000000000000000 ) ;
#646 = LINE ( 'NONE', #13977, #4274 ) ;
#647 = CARTESIAN_POINT ( 'NONE',  ( -0.8561741729129465073, 61.93301270000000613, 48.30000000109247082 ) ) ;
#648 = DIRECTION ( 'NONE',  ( -0.000000000000000000, -1.000000000000000000, -0.000000000000000000 ) ) ;
#649 = VECTOR ( 'NONE', #15920, 1000.000000000000000 ) ;
#650 = ORIENTED_EDGE ( 'NONE', *, *, #9548, .F. ) ;
#651 = CARTESIAN_POINT ( 'NONE',  ( -15.16482700510264436, -16.99999999999997868, 37.73632249208302625 ) ) ;
#652 = CIRCLE ( 'NONE', #5974, 2.999999999999999112 ) ;
#653 =( LENGTH_UNIT ( ) NAMED_UNIT ( * ) SI_UNIT ( .MILLI., .METRE. ) );
#654 = EDGE_CURVE ( 'NONE', #10863, #8734, #2898, .T. ) ;
#655 = LINE ( 'NONE', #6643, #5310 ) ;
#656 = EDGE_CURVE ( 'NONE', #10380, #10947, #3089, .T. ) ;
#657 = CARTESIAN_POINT ( 'NONE',  ( -17.68048971390461688, -25.35725562635141372, 34.01367750791696665 ) ) ;
#658 = FACE_OUTER_BOUND ( 'NONE', #6966, .T. ) ;
#659 = EDGE_CURVE ( 'NONE', #16948, #10794, #10433, .T. ) ;
#660 = CARTESIAN_POINT ( 'NONE',  ( -18.64274437364860049, -18.02023567606023491, 21.54882249208304046 ) ) ;
#661 = VECTOR ( 'NONE', #3719, 1000.000000000000000 ) ;
#662 = CARTESIAN_POINT ( 'NONE',  ( 0.8561741729129460632, 66.06698729999999387, 46.90000000109247225 ) ) ;
#663 = VERTEX_POINT ( 'NONE', #14958 ) ;
#664 = EDGE_LOOP ( 'NONE', ( #7813, #9877, #10932, #13103 ) ) ;
#665 = EDGE_CURVE ( 'NONE', #4048, #8707, #8409, .T. ) ;
#666 = CARTESIAN_POINT ( 'NONE',  ( 5.799999999999985612, 29.65425233947092920, 56.47747564417436195 ) ) ;
#667 = CARTESIAN_POINT ( 'NONE',  ( -41.00000000000000711, 110.0000000000000000, -32.00000000000000000 ) ) ;
#668 = VECTOR ( 'NONE', #17005, 1000.000000000000000 ) ;
#669 = CARTESIAN_POINT ( 'NONE',  ( 2.066987300000001859, 63.14382582708704916, 49.10000000109246088 ) ) ;
#670 = CARTESIAN_POINT ( 'NONE',  ( -25.00000000000000000, 110.0000000000000000, 30.00000000000000000 ) ) ;
#671 = COLOUR_RGB ( '', 0.72549020, 0.75294118, 0.79215686) ;
#672 = DIRECTION ( 'NONE',  ( -0.000000000000000000, -0.7071067811865456854, -0.7071067811865493491 ) ) ;
#673 = PLANE ( 'NONE',  #15685 ) ;
#674 = CIRCLE ( 'NONE', #11604, 7.000000000000001776 ) ;
#675 = DIRECTION ( 'NONE',  ( -1.000000000000000000, 0.000000000000000000, -2.081668171172167774E-16 ) ) ;
#676 = EDGE_CURVE ( 'NONE', #9708, #9275, #13573, .T. ) ;
#677 = VERTEX_POINT ( 'NONE', #10628 ) ;
#678 = ORIENTED_EDGE ( 'NONE', *, *, #14772, .F. ) ;
#679 = CARTESIAN_POINT ( 'NONE',  ( -18.35725562635144925, -17.85540867095761186, 24.82617750791695599 ) ) ;
#680 =( NAMED_UNIT ( * ) PLANE_ANGLE_UNIT ( ) SI_UNIT ( $, .RADIAN. ) );
#681 = ORIENTED_EDGE ( 'NONE', *, *, #18605, .T. ) ;
#683 = EDGE_LOOP ( 'NONE', ( #8801, #8791, #6089, #8526 ) ) ;
#682 = ORIENTED_EDGE ( 'NONE', *, *, #6769, .F. ) ;
#684 = CARTESIAN_POINT ( 'NONE',  ( -17.99999999999999645, -24.16482700510260173, 31.17382249208304046 ) ) ;
#685 = CARTESIAN_POINT ( 'NONE',  ( -18.35725562635144925, -17.85540867095761186, 19.57617750791695954 ) ) ;
#686 = FACE_BOUND ( 'NONE', #17329, .T. ) ;
#687 = CARTESIAN_POINT ( 'NONE',  ( 2.500000000000001776, 64.00000000000000000, 47.30000000218494449 ) ) ;
#688 = DIRECTION ( 'NONE',  ( 0.000000000000000000, 0.4999999999999991673, -0.8660254037844391517 ) ) ;
#689 = ORIENTED_EDGE ( 'NONE', *, *, #866, .F. ) ;
#690 = CARTESIAN_POINT ( 'NONE',  ( -16.64274437364856496, -26.51566270880199738, 28.32617750791696665 ) ) ;
#691 = DIRECTION ( 'NONE',  ( 0.000000000000000000, -1.000000000000000000, -0.000000000000000000 ) ) ;
#692 = ORIENTED_EDGE ( 'NONE', *, *, #7602, .T. ) ;
#693 = CARTESIAN_POINT ( 'NONE',  ( -1.040834085586084257E-14, 29.03553390593270578, 56.03553390593273775 ) ) ;
#694 = ORIENTED_EDGE ( 'NONE', *, *, #13084, .T. ) ;
#695 = CARTESIAN_POINT ( 'NONE',  ( -41.00000000000000711, 110.0000000000000000, -5.000000000000000888 ) ) ;
#696 = PRODUCT_RELATED_PRODUCT_CATEGORY ( 'part', '', ( #5998 ) ) ;
#697 =( REPRESENTATION_RELATIONSHIP ('NONE','NONE', #7912, #8522 ) REPRESENTATION_RELATIONSHIP_WITH_TRANSFORMATION ( #9131 )SHAPE_REPRESENTATION_RELATIONSHIP( ) );
#698 = CARTESIAN_POINT ( 'NONE',  ( 0.000000000000000000, 0.000000000000000000, -50.00000000000000000 ) ) ;
#699 = LINE ( 'NONE', #15785, #15320 ) ;
#700 = CARTESIAN_POINT ( 'NONE',  ( -1.265664690411616068E-16, 66.06698730000000808, 48.55000000109247082 ) ) ;
#701 = CARTESIAN_POINT ( 'NONE',  ( -2.066987300000001415, 64.85617417291294373, 49.70000000109247651 ) ) ;
#702 = FACE_OUTER_BOUND ( 'NONE', #9718, .T. ) ;
#703 = AXIS2_PLACEMENT_3D ( 'NONE', #5641, #5740, #11602 ) ;
#704 = CARTESIAN_POINT ( 'NONE',  ( -4.012354697599906928, 32.70432772728319293, 53.78000129688592068 ) ) ;
#705 = CARTESIAN_POINT ( 'NONE',  ( -0.1250000000000104083, 31.97002704785689531, 54.16170093578840294 ) ) ;
#706 = EDGE_CURVE ( 'NONE', #9890, #18408, #2462, .T. ) ;
#707 = ORIENTED_EDGE ( 'NONE', *, *, #2186, .T. ) ;
#708 = CARTESIAN_POINT ( 'NONE',  ( -20.04416526290808065, -25.17491895705300209, 34.23242750791695954 ) ) ;
#709 = LINE ( 'NONE', #13739, #8347 ) ;
#710 = ORIENTED_EDGE ( 'NONE', *, *, #11906, .T. ) ;
#711 = CARTESIAN_POINT ( 'NONE',  ( -14.83517299489735741, -28.99999999999998224, 29.86132249208304401 ) ) ;
#712 = LINE ( 'NONE', #8437, #14065 ) ;
#713 = CARTESIAN_POINT ( 'NONE',  ( -17.31681416490117087, -21.92450931948788551, 26.58007249208304756 ) ) ;
#714 = DIRECTION ( 'NONE',  ( -1.000000000000000000, 0.000000000000000000, -0.000000000000000000 ) ) ;
#715 = ORIENTED_EDGE ( 'NONE', *, *, #16980, .F. ) ;
#716 = CARTESIAN_POINT ( 'NONE',  ( -2.492551403682565780, 31.20336399182265552, 54.92836399182263563 ) ) ;
#717 = VERTEX_POINT ( 'NONE', #15447 ) ;
#718 = LINE ( 'NONE', #13034, #5625 ) ;
#719 = CARTESIAN_POINT ( 'NONE',  ( -1.035533905932738863, 61.50000000000000000, 46.14999999999999858 ) ) ;
#720 = CARTESIAN_POINT ( 'NONE',  ( -2.500000000000001776, 64.00000000000000000, 46.10000000218494165 ) ) ;
#721 = CARTESIAN_POINT ( 'NONE',  ( 2.500000000000000000, 3.004629197474319246E-15, 2.042000000000000259 ) ) ;
#722 = LINE ( 'NONE', #6702, #12252 ) ;
#723 = CARTESIAN_POINT ( 'NONE',  ( 1.300000000000000044, -1.478016689125442706, 1.843143693225357538E-15 ) ) ;
#724 = PLANE ( 'NONE',  #16794 ) ;
#725 = ADVANCED_FACE ( 'NONE', ( #16824 ), #4868, .T. ) ;
#726 = ORIENTED_EDGE ( 'NONE', *, *, #2307, .T. ) ;
#727 = CARTESIAN_POINT ( 'NONE',  ( -18.53959229564986799, -20.21908421996107563, 29.85742750791695599 ) ) ;
#728 = CARTESIAN_POINT ( 'NONE',  ( -1.461580736456473462, 62.53841926354353120, 48.85000000109246798 ) ) ;
#729 = CARTESIAN_POINT ( 'NONE',  ( -17.64274437364858983, -19.75228648362910633, 26.79882249208304401 ) ) ;
#730 = DIRECTION ( 'NONE',  ( -1.000000000000000000, 0.000000000000000000, 0.000000000000000000 ) ) ;
#731 = CARTESIAN_POINT ( 'NONE',  ( -10.04416526290807710, -25.50457296725819489, 26.79492750791695954 ) ) ;
#732 = ADVANCED_FACE ( 'NONE', ( #1925 ), #15252, .T. ) ;
#733 = CARTESIAN_POINT ( 'NONE',  ( -40.00000000000000000, 53.00000000000000711, 13.50000000000000000 ) ) ;
#734 = CARTESIAN_POINT ( 'NONE',  ( -17.35725562635144215, -19.58745947852648683, 35.32617750791695954 ) ) ;
#735 = DIRECTION ( 'NONE',  ( 0.000000000000000000, 0.000000000000000000, -1.000000000000000000 ) ) ;
#736 = CARTESIAN_POINT ( 'NONE',  ( -12.35725562635140307, -28.24771351637085459, 24.17382249208304046 ) ) ;
#737 = CARTESIAN_POINT ( 'NONE',  ( 1.461580736456473684, 65.46158073645646880, 45.45000000109246940 ) ) ;
#738 = CARTESIAN_POINT ( 'NONE',  ( -41.00000000000000711, 53.00000000000000711, -19.00000000000000000 ) ) ;
#739 = DIRECTION ( 'NONE',  ( 0.000000000000000000, -1.000000000000000000, 0.000000000000000000 ) ) ;
#740 = CARTESIAN_POINT ( 'NONE',  ( -2.500000000000001776, 64.00000000000000000, 48.50000000218494023 ) ) ;
#741 = CARTESIAN_POINT ( 'NONE',  ( 2.066987300000001859, 64.85617417291294373, 46.20000000109247651 ) ) ;
#742 = DIRECTION ( 'NONE',  ( -1.000000000000000000, 2.720046410331633524E-15, -2.220446049250313081E-15 ) ) ;
#743 = ORIENTED_EDGE ( 'NONE', *, *, #13910, .T. ) ;
#744 = EDGE_CURVE ( 'NONE', #4631, #8350, #8098, .T. ) ;
#745 = CARTESIAN_POINT ( 'NONE',  ( -1.461580736456473462, 62.53841926354353120, 46.45000000109246940 ) ) ;
#746 = CARTESIAN_POINT ( 'NONE',  ( -16.35725562635142794, -21.31951028609535470, 30.07617750791696309 ) ) ;
#747 = CARTESIAN_POINT ( 'NONE',  ( 0.000000000000000000, 0.000000000000000000, 3.000000000000000000 ) ) ;
#748 = CARTESIAN_POINT ( 'NONE',  ( -9.996306089212408708, -18.75498260482328661, 38.39257249208304756 ) ) ;
#749 = CARTESIAN_POINT ( 'NONE',  ( 2.066987300000002303, 63.14382582708705627, 45.90000000109247225 ) ) ;
#750 = ORIENTED_EDGE ( 'NONE', *, *, #15854, .T. ) ;
#751 = FACE_OUTER_BOUND ( 'NONE', #949, .T. ) ;
#752 = CARTESIAN_POINT ( 'NONE',  ( -1.485306817036799787, -32.50000000000000711, -3.000000000000000000 ) ) ;
#753 = CARTESIAN_POINT ( 'NONE',  ( -0.8561741729129466183, 61.93301270000000613, 45.70000000109248361 ) ) ;
#754 = DIRECTION ( 'NONE',  ( 1.000000000000000000, 0.000000000000000000, 0.000000000000000000 ) ) ;
#755 = DIRECTION ( 'NONE',  ( 0.000000000000000000, 0.000000000000000000, -1.000000000000000000 ) ) ;
#756 = EDGE_CURVE ( 'NONE', #8924, #4687, #13097, .T. ) ;
#757 = EDGE_CURVE ( 'NONE', #10804, #4598, #9265, .T. ) ;
#758 = VECTOR ( 'NONE', #9249, 1000.000000000000000 ) ;
#759 = DIRECTION ( 'NONE',  ( 1.000000000000000000, -0.000000000000000000, -0.000000000000000000 ) ) ;
#760 = EDGE_CURVE ( 'NONE', #2931, #1646, #7705, .T. ) ;
#761 = CARTESIAN_POINT ( 'NONE',  ( -2.499999999999998668, 62.96446609406726225, 47.64999999999999858 ) ) ;
#762 = EDGE_LOOP ( 'NONE', ( #16079, #7445, #9963, #6983 ) ) ;
#763 = VERTEX_POINT ( 'NONE', #6340 ) ;
#764 = CARTESIAN_POINT ( 'NONE',  ( -20.00369391078762860, -18.75498260482333279, 24.60742750791696309 ) ) ;
#765 = ORIENTED_EDGE ( 'NONE', *, *, #8549, .F. ) ;
#767 = ORIENTED_EDGE ( 'NONE', *, *, #16915, .F. ) ;
#766 = ORIENTED_EDGE ( 'NONE', *, *, #2307, .F. ) ;
#768 = CARTESIAN_POINT ( 'NONE',  ( -12.48433729119799196, -22.35725562635139596, 28.11132249208304401 ) ) ;
#769 = CARTESIAN_POINT ( 'NONE',  ( -9.020235676060220698, -27.64274437364852588, 16.51367750791695954 ) ) ;
#770 = COLOUR_RGB ( '', 0.09019608, 0.27058824, 0.51372549) ;
#771 = CARTESIAN_POINT ( 'NONE',  ( 1.035533905932738197, 66.50000000000000000, 47.34999999999998721 ) ) ;
#772 = CARTESIAN_POINT ( 'NONE',  ( -2.500000000000001776, 64.00000000000000000, 48.50000000218494023 ) ) ;
#773 = LINE ( 'NONE', #2428, #11566 ) ;
#774 = ORIENTED_EDGE ( 'NONE', *, *, #620, .F. ) ;
#775 = CARTESIAN_POINT ( 'NONE',  ( -13.64274437364856141, -26.68048971390460622, 32.70117750791696665 ) ) ;
#776 = DIRECTION ( 'NONE',  ( 1.000000000000000000, -0.000000000000000000, -0.000000000000000000 ) ) ;
#777 = ORIENTED_EDGE ( 'NONE', *, *, #13586, .F. ) ;
#778 = DIRECTION ( 'NONE',  ( 0.000000000000000000, -1.000000000000000000, 0.000000000000000000 ) ) ;
#779 = ORIENTED_EDGE ( 'NONE', *, *, #9790, .T. ) ;
#780 = CARTESIAN_POINT ( 'NONE',  ( -43.50000000000000000, 2.999000000000001442, 32.50000000000000000 ) ) ;
#781 = ADVANCED_FACE ( 'NONE', ( #18300 ), #17023, .F. ) ;
#782 = DIRECTION ( 'NONE',  ( -0.000000000000000000, -0.000000000000000000, -1.000000000000000000 ) ) ;
#783 = CARTESIAN_POINT ( 'NONE',  ( -40.00000000000000711, 113.0000000000000000, 6.999999999999999112 ) ) ;
#784 = CARTESIAN_POINT ( 'NONE',  ( 2.066987300000002303, 63.14382582708705627, 45.10000000109246798 ) ) ;
#785 = ADVANCED_FACE ( 'NONE', ( #639 ), #6236, .F. ) ;
#786 = CARTESIAN_POINT ( 'NONE',  ( 1.461580736456473906, 62.53841926354353120, 48.45000000109246940 ) ) ;
#787 = DIRECTION ( 'NONE',  ( 0.000000000000000000, 1.000000000000000000, 0.000000000000000000 ) ) ;
#788 = AXIS2_PLACEMENT_3D ( 'NONE', #4564, #344, #9345 ) ;
#789 = FACE_OUTER_BOUND ( 'NONE', #10775, .T. ) ;
#790 = AXIS2_PLACEMENT_3D ( 'NONE', #8176, #5235, #14146 ) ;
#791 = PLANE ( 'NONE',  #8315 ) ;
#792 = ORIENTED_EDGE ( 'NONE', *, *, #7610, .F. ) ;
#793 = VERTEX_POINT ( 'NONE', #18588 ) ;
#794 = CARTESIAN_POINT ( 'NONE',  ( -16.17491895705301275, -18.95583473709189803, 30.29492750791695244 ) ) ;
#795 = DIRECTION ( 'NONE',  ( -0.000000000000000000, -1.000000000000000000, -0.000000000000000000 ) ) ;
#796 = ORIENTED_EDGE ( 'NONE', *, *, #8690, .T. ) ;
#797 = CARTESIAN_POINT ( 'NONE',  ( -19.24771351637086880, -26.64274437364857206, 25.48632249208304401 ) ) ;
#798 = LINE ( 'NONE', #18747, #17206 ) ;
#799 = CARTESIAN_POINT ( 'NONE',  ( -17.95583473709190869, -24.96867458239598037, 36.20507249208304756 ) ) ;
#800 = CARTESIAN_POINT ( 'NONE',  ( 0.000000000000000000, 1.178949249685212974, -2.042000000000001148 ) ) ;
#801 = ORIENTED_EDGE ( 'NONE', *, *, #13567, .F. ) ;
#802 = VECTOR ( 'NONE', #3506, 1000.000000000000000 ) ;
#803 = CARTESIAN_POINT ( 'NONE',  ( -41.00000000000000711, 110.0000000000000000, -5.000000000000000888 ) ) ;
#804 = ORIENTED_EDGE ( 'NONE', *, *, #13435, .F. ) ;
#805 = EDGE_CURVE ( 'NONE', #14571, #4512, #3295, .T. ) ;
#806 = DIRECTION ( 'NONE',  ( 1.000000000000000000, 0.000000000000000000, 0.000000000000000000 ) ) ;
#807 = FACE_OUTER_BOUND ( 'NONE', #12482, .T. ) ;
#808 = DIRECTION ( 'NONE',  ( -0.000000000000000000, -0.000000000000000000, -1.000000000000000000 ) ) ;
#809 = CARTESIAN_POINT ( 'NONE',  ( -41.00000000000000711, 113.0000000000000000, 30.00000000000000000 ) ) ;
#810 = EDGE_CURVE ( 'NONE', #15519, #4628, #9647, .T. ) ;
#811 = SURFACE_SIDE_STYLE ('',( #2189 ) ) ;
#812 = DIRECTION ( 'NONE',  ( 0.7071067811865463515, 0.000000000000000000, -0.7071067811865487940 ) ) ;
#813 = VECTOR ( 'NONE', #8589, 1000.000000000000000 ) ;
#814 = CARTESIAN_POINT ( 'NONE',  ( -45.00000000000000000, 6.000000000000000000, 56.49999999999998579 ) ) ;
#815 = AXIS2_PLACEMENT_3D ( 'NONE', #12603, #5162, #11125 ) ;
#816 = ORIENTED_EDGE ( 'NONE', *, *, #9598, .T. ) ;
#817 = CARTESIAN_POINT ( 'NONE',  ( -18.53959229564986799, -20.21908421996107563, 35.10742750791694533 ) ) ;
#818 = CARTESIAN_POINT ( 'NONE',  ( -0.8561741729129465073, 61.93301270000000613, 46.50000000109247367 ) ) ;
#819 = CARTESIAN_POINT ( 'NONE',  ( -16.17491895705296656, -29.04416526290807710, 30.08007249208304401 ) ) ;
#820 = DIRECTION ( 'NONE',  ( 0.000000000000000000, 0.000000000000000000, 1.000000000000000000 ) ) ;
#821 = EDGE_CURVE ( 'NONE', #5173, #12630, #4675, .T. ) ;
#822 = CARTESIAN_POINT ( 'NONE',  ( -16.17491895705301275, -18.95583473709189803, 35.54492750791695954 ) ) ;
#823 = FACE_OUTER_BOUND ( 'NONE', #4002, .T. ) ;
#824 = VECTOR ( 'NONE', #2637, 1000.000000000000000 ) ;
#825 = CARTESIAN_POINT ( 'NONE',  ( -20.04416526290808065, -25.17491895705300209, 34.23242750791696665 ) ) ;
#826 = LINE ( 'NONE', #14446, #4346 ) ;
#827 = CARTESIAN_POINT ( 'NONE',  ( -20.04416526290809131, -22.82508104294700502, 31.39257249208304046 ) ) ;
#828 = CIRCLE ( 'NONE', #10842, 2.500000000000000444 ) ;
#829 = CARTESIAN_POINT ( 'NONE',  ( -1.767766952966370209, 65.76776695296638309, 48.29999999999999716 ) ) ;
#830 = CARTESIAN_POINT ( 'NONE',  ( -50.00000000000002132, 0.000000000000000000, -60.00000000000002132 ) ) ;
#831 = LINE ( 'NONE', #11312, #7741 ) ;
#832 = CARTESIAN_POINT ( 'NONE',  ( -2.500000000000000888, 62.96446609406726935, 48.44999999999999574 ) ) ;
#833 = DIRECTION ( 'NONE',  ( -0.000000000000000000, -0.000000000000000000, -1.000000000000000000 ) ) ;
#834 = VERTEX_POINT ( 'NONE', #18496 ) ;
#835 = SURFACE_STYLE_FILL_AREA ( #11035 ) ;
#836 = VECTOR ( 'NONE', #15353, 1000.000000000000000 ) ;
#837 = CARTESIAN_POINT ( 'NONE',  ( 1.461580736456473906, 62.53841926354353120, 46.65000000109247225 ) ) ;
#838 = CARTESIAN_POINT ( 'NONE',  ( -11.95583473709191047, -23.36097942780921954, 36.85742750791697375 ) ) ;
#839 = CARTESIAN_POINT ( 'NONE',  ( 2.500000000000001776, 64.00000000000000000, 48.79999999999999716 ) ) ;
#840 = CARTESIAN_POINT ( 'NONE',  ( -18.64274437364860049, -18.02023567606023491, 26.79882249208304401 ) ) ;
#841 = CARTESIAN_POINT ( 'NONE',  ( -1.461580736456473906, 65.46158073645646880, 47.05000000109247082 ) ) ;
#842 = ORIENTED_EDGE ( 'NONE', *, *, #15989, .T. ) ;
#843 = FACE_OUTER_BOUND ( 'NONE', #12229, .T. ) ;
#844 = CYLINDRICAL_SURFACE ( 'NONE', #14759, 6.799999999999997158 ) ;
#845 = CARTESIAN_POINT ( 'NONE',  ( -1.265664690411616068E-16, 66.06698730000000808, 46.95000000109246940 ) ) ;
#846 = DIRECTION ( 'NONE',  ( 0.000000000000000000, 0.000000000000000000, 1.000000000000000000 ) ) ;
#847 = EDGE_CURVE ( 'NONE', #14186, #5501, #5607, .T. ) ;
#848 = EDGE_CURVE ( 'NONE', #5969, #14590, #7908, .T. ) ;
#849 = CARTESIAN_POINT ( 'NONE',  ( 2.500000000000001776, 64.00000000000000000, 47.99999999999999289 ) ) ;
#850 = CARTESIAN_POINT ( 'NONE',  ( -12.50000000000000000, -35.50000000000000000, 5.500000000000000000 ) ) ;
#851 = EDGE_CURVE ( 'NONE', #13992, #16279, #14676, .T. ) ;
#852 = LINE ( 'NONE', #17325, #17405 ) ;
#853 = VERTEX_POINT ( 'NONE', #2582 ) ;
#854 = EDGE_LOOP ( 'NONE', ( #12884, #7574 ) ) ;
#855 = CARTESIAN_POINT ( 'NONE',  ( -16.71081734191520596, -31.04416526290808065, 3.830072492083039126 ) ) ;
#856 = VERTEX_POINT ( 'NONE', #12774 ) ;
#858 = ORIENTED_EDGE ( 'NONE', *, *, #9631, .T. ) ;
#857 = ORIENTED_EDGE ( 'NONE', *, *, #3921, .T. ) ;
#859 = CARTESIAN_POINT ( 'NONE',  ( -12.92450931948790149, -21.68318583509881137, 27.89257249208304401 ) ) ;
#860 = CARTESIAN_POINT ( 'NONE',  ( -8.855408670957631401, -20.64274437364852943, 26.13867750791696309 ) ) ;
#861 = EDGE_CURVE ( 'NONE', #12841, #2217, #5438, .T. ) ;
#862 = LINE ( 'NONE', #12814, #6940 ) ;
#863 = CARTESIAN_POINT ( 'NONE',  ( -1.530808498934192803E-16, 66.50000000000000000, 49.10000000218494165 ) ) ;
#864 = CARTESIAN_POINT ( 'NONE',  ( -41.00000000000000711, 110.0000000000000000, 21.00000000000000000 ) ) ;
#865 = ORIENTED_EDGE ( 'NONE', *, *, #15879, .F. ) ;
#866 = EDGE_CURVE ( 'NONE', #19283, #17238, #6714, .T. ) ;
#867 = EDGE_CURVE ( 'NONE', #15167, #11814, #11394, .T. ) ;
#868 = PLANE ( 'NONE',  #16631 ) ;
#869 = VERTEX_POINT ( 'NONE', #11305 ) ;
#870 = FACE_OUTER_BOUND ( 'NONE', #10505, .T. ) ;
#871 = ORIENTED_EDGE ( 'NONE', *, *, #3155, .F. ) ;
#872 = DIRECTION ( 'NONE',  ( 0.5773502691896360561, 0.8164965809277188180, 0.000000000000000000 ) ) ;
#873 = PLANE ( 'NONE',  #1854 ) ;
#874 = PLANE ( 'NONE',  #924 ) ;
#875 = CARTESIAN_POINT ( 'NONE',  ( -1.461580736456473906, 65.46158073645646880, 47.05000000109247082 ) ) ;
#876 = EDGE_CURVE ( 'NONE', #15646, #8090, #3962, .T. ) ;
#877 = CARTESIAN_POINT ( 'NONE',  ( 0.000000000000000000, 0.000000000000000000, 0.000000000000000000 ) ) ;
#878 = CARTESIAN_POINT ( 'NONE',  ( -6.528048594804060301, -45.28611686177728046, 3.000000000000000000 ) ) ;
#879 = LINE ( 'NONE', #8340, #1099 ) ;
#880 = ORIENTED_EDGE ( 'NONE', *, *, #12234, .F. ) ;
#881 = ORIENTED_EDGE ( 'NONE', *, *, #9499, .T. ) ;
#882 = CARTESIAN_POINT ( 'NONE',  ( -17.64274437364855430, -28.24771351637087236, 33.57617750791696665 ) ) ;
#883 = VECTOR ( 'NONE', #3984, 1000.000000000000000 ) ;
#884 = PLANE ( 'NONE',  #9599 ) ;
#885 = VERTEX_POINT ( 'NONE', #10021 ) ;
#886 = CARTESIAN_POINT ( 'NONE',  ( -20.04416526290809131, -22.82508104294699791, 26.14257249208303691 ) ) ;
#887 = EDGE_CURVE ( 'NONE', #16466, #19197, #4055, .T. ) ;
#888 = EDGE_CURVE ( 'NONE', #7059, #18716, #5252, .T. ) ;
#889 = CARTESIAN_POINT ( 'NONE',  ( 0.1249999999999895917, 27.16170093578836031, 58.97002704785691662 ) ) ;
#890 = EDGE_LOOP ( 'NONE', ( #5514, #15277, #16400, #16858 ) ) ;
#891 = CARTESIAN_POINT ( 'NONE',  ( -17.51566270880199738, -25.64274437364856496, 35.98632249208304756 ) ) ;
#892 = DIRECTION ( 'NONE',  ( 0.000000000000000000, 0.8660254037844380415, -0.5000000000000012212 ) ) ;
#893 = EDGE_LOOP ( 'NONE', ( #6187, #11365, #9315, #5304 ) ) ;
#894 = DIRECTION ( 'NONE',  ( 0.000000000000000000, 0.000000000000000000, -1.000000000000000000 ) ) ;
#895 = VERTEX_POINT ( 'NONE', #3865 ) ;
#896 = CARTESIAN_POINT ( 'NONE',  ( -47.00000000000001421, 118.0000000000000142, 56.99999999999997158 ) ) ;
#897 = ADVANCED_FACE ( 'NONE', ( #8562 ), #18770, .T. ) ;
#898 = CARTESIAN_POINT ( 'NONE',  ( -21.50000000000000000, 115.0000000000000000, -52.50000000000000711 ) ) ;
#899 = CARTESIAN_POINT ( 'NONE',  ( 41.99999999999997868, 3.000000000000000000, 51.99999999999997868 ) ) ;
#900 = CARTESIAN_POINT ( 'NONE',  ( -16.17491895705301275, -18.95583473709189803, 30.29492750791695244 ) ) ;
#901 = SURFACE_STYLE_USAGE ( .BOTH. , #5326 ) ;
#902 = DIRECTION ( 'NONE',  ( -0.000000000000000000, -1.000000000000000000, -0.000000000000000000 ) ) ;
#903 = DIRECTION ( 'NONE',  ( 1.000000000000000000, -7.410738689372937262E-15, 7.410738689372897819E-15 ) ) ;
#904 = VECTOR ( 'NONE', #4505, 1000.000000000000000 ) ;
#905 = CARTESIAN_POINT ( 'NONE',  ( -15.00000000000000000, 50.00000000000000000, 30.00000000000000000 ) ) ;
#906 = EDGE_LOOP ( 'NONE', ( #5274, #17895, #7595, #10353 ) ) ;
#907 = ADVANCED_FACE ( 'NONE', ( #15824 ), #16023, .F. ) ;
#908 = VERTEX_POINT ( 'NONE', #18961 ) ;
#909 = CIRCLE ( 'NONE', #3424, 1.500000000000001332 ) ;
#910 = CARTESIAN_POINT ( 'NONE',  ( -20.04416526290808065, -25.17491895705300209, 28.98242750791695244 ) ) ;
#911 = CARTESIAN_POINT ( 'NONE',  ( 2.066987300000002303, 63.14382582708705627, 49.10000000109246088 ) ) ;
#912 = CARTESIAN_POINT ( 'NONE',  ( -10.58745947852648328, -26.35725562635138530, 28.98632249208304401 ) ) ;
#913 = LINE ( 'NONE', #17382, #14105 ) ;
#914 = DIRECTION ( 'NONE',  ( 1.000000000000000000, -2.665111688417744333E-15, 2.272588573746785565E-15 ) ) ;
#915 = CARTESIAN_POINT ( 'NONE',  ( -13.49542703274178379, -19.04416526290806289, 30.73242750791695599 ) ) ;
#916 = LINE ( 'NONE', #1204, #4548 ) ;
#918 = CARTESIAN_POINT ( 'NONE',  ( -10.58745947852649927, -21.64274437364853654, 26.13867750791695599 ) ) ;
#917 = AXIS2_PLACEMENT_3D ( 'NONE', #6913, #14180, #12886 ) ;
#919 = DIRECTION ( 'NONE',  ( -0.000000000000000000, 1.000000000000000000, 1.224646799147353207E-16 ) ) ;
#920 = CARTESIAN_POINT ( 'NONE',  ( -0.9999999999999945599, -28.00000000000000000, 9.500000000000001776 ) ) ;
#921 = CARTESIAN_POINT ( 'NONE',  ( -0.8561741729129465073, 61.93301270000000613, 45.10000000109246798 ) ) ;
#922 = DIRECTION ( 'NONE',  ( 0.000000000000000000, 1.000000000000000000, 0.000000000000000000 ) ) ;
#923 = VECTOR ( 'NONE', #18178, 1000.000000000000000 ) ;
#924 = AXIS2_PLACEMENT_3D ( 'NONE', #9416, #11075, #6488 ) ;
#925 = CARTESIAN_POINT ( 'NONE',  ( -2.500000000000001776, 64.00000000000000000, 48.50000000218494023 ) ) ;
#926 = CARTESIAN_POINT ( 'NONE',  ( 2.500000000000002220, 62.96446609406726935, 49.54999999999999716 ) ) ;
#927 = CARTESIAN_POINT ( 'NONE',  ( -41.00000000000000711, 110.0000000000000000, 14.50000000000000000 ) ) ;
#928 = VECTOR ( 'NONE', #4321, 1000.000000000000000 ) ;
#929 = EDGE_LOOP ( 'NONE', ( #4729, #17644, #6889, #19102, #1362, #1856, #1672, #7418 ) ) ;
#930 = SHAPE_REPRESENTATION_RELATIONSHIP ( 'NONE' , 'NONE' ,  #3576, #11772 ) ;
#931 = CARTESIAN_POINT ( 'NONE',  ( -2.066987300000001415, 64.00000000000000000, 45.55000000109246372 ) ) ;
#932 = AXIS2_PLACEMENT_3D ( 'NONE', #16950, #3411, #7830 ) ;
#933 = CARTESIAN_POINT ( 'NONE',  ( -17.35725562635144215, -19.58745947852648683, 3.826177507916958209 ) ) ;
#934 = PLANE ( 'NONE',  #16670 ) ;
#935 = CARTESIAN_POINT ( 'NONE',  ( -9.754982604823302594, -29.00369391078756465, 34.45507249208304046 ) ) ;
#936 = AXIS2_PLACEMENT_3D ( 'NONE', #14392, #3821, #15873 ) ;
#937 = CARTESIAN_POINT ( 'NONE',  ( 1.461580736456473906, 62.53841926354353120, 49.25000000109246656 ) ) ;
#938 = EDGE_LOOP ( 'NONE', ( #12819, #19041, #5593, #2064 ) ) ;
#939 = CARTESIAN_POINT ( 'NONE',  ( 2.500000000000000000, -1.178949249685214307, 2.042000000000002036 ) ) ;
#940 = DIRECTION ( 'NONE',  ( 1.000000000000000000, 1.156482317317871478E-16, -0.000000000000000000 ) ) ;
#941 = VECTOR ( 'NONE', #1797, 1000.000000000000000 ) ;
#942 = CARTESIAN_POINT ( 'NONE',  ( 2.066987300000001415, 64.00000000000000000, 47.55000000109247082 ) ) ;
#943 = LINE ( 'NONE', #17412, #883 ) ;
#944 = FACE_OUTER_BOUND ( 'NONE', #1471, .T. ) ;
#945 = AXIS2_PLACEMENT_3D ( 'NONE', #1086, #16280, #1182 ) ;
#946 = DIRECTION ( 'NONE',  ( 0.000000000000000000, -1.000000000000000000, 0.000000000000000000 ) ) ;
#947 = VECTOR ( 'NONE', #14495, 1000.000000000000000 ) ;
#948 = PLANE ( 'NONE',  #3329 ) ;
#949 = EDGE_LOOP ( 'NONE', ( #17084, #14289, #6599, #2912 ) ) ;
#950 = ORIENTED_EDGE ( 'NONE', *, *, #18620, .F. ) ;
#951 = CARTESIAN_POINT ( 'NONE',  ( -12.95952864787948755, -30.95583473709188382, 8.642572492083038682 ) ) ;
#952 = FILL_AREA_STYLE_COLOUR ( '', #15246 ) ;
#953 = ORIENTED_EDGE ( 'NONE', *, *, #2641, .T. ) ;
#955 = ORIENTED_EDGE ( 'NONE', *, *, #6127, .F. ) ;
#954 = ORIENTED_EDGE ( 'NONE', *, *, #9245, .F. ) ;
#956 = CARTESIAN_POINT ( 'NONE',  ( -13.64274437364856141, -26.68048971390460622, 6.451177507916961318 ) ) ;
#957 = EDGE_CURVE ( 'NONE', #15953, #1682, #18392, .T. ) ;
#958 = EDGE_CURVE ( 'NONE', #6376, #15290, #14540, .T. ) ;
#959 = CARTESIAN_POINT ( 'NONE',  ( -7.999999999999996447, -24.16482700510256976, 31.82617750791695954 ) ) ;
#960 = VECTOR ( 'NONE', #4995, 1000.000000000000000 ) ;
#961 = LINE ( 'NONE', #13293, #11013 ) ;
#962 = CARTESIAN_POINT ( 'NONE',  ( -1.767766952966369765, 62.23223304703363112, 47.00000000218494733 ) ) ;
#963 = DIRECTION ( 'NONE',  ( 0.000000000000000000, 0.000000000000000000, -1.000000000000000000 ) ) ;
#964 = VERTEX_POINT ( 'NONE', #8284 ) ;
#965 = EDGE_CURVE ( 'NONE', #11814, #8458, #14994, .T. ) ;
#966 =( BOUNDED_CURVE ( )  B_SPLINE_CURVE ( 2, ( #11278, #18750, #6971, #15996, #1084, #12938, #18933, #13032, #5598 ),
 .UNSPECIFIED., .F., .F. ) 
 B_SPLINE_CURVE_WITH_KNOTS ( ( 3, 2, 2, 2, 3 ),
 ( 0.4285714285714284366, 0.4464285714285713413, 0.4642857142857141906, 0.4821428571428570953, 0.4999999999999999445 ),
 .UNSPECIFIED. ) 
 CURVE ( )  GEOMETRIC_REPRESENTATION_ITEM ( )  RATIONAL_B_SPLINE_CURVE ( ( 1.000000000000000444, 0.9238795325112862944, 1.000000000000000000, 0.9238795325112867385, 1.000000000000000000, 0.9238795325112867385, 1.000000000000000000, 0.9238795325112869605, 0.9999999999999997780 ) ) 
 REPRESENTATION_ITEM ( '' )  );
#967 = AXIS2_PLACEMENT_3D ( 'NONE', #13487, #8976, #17705 ) ;
#968 = FACE_OUTER_BOUND ( 'NONE', #890, .T. ) ;
#969 = ORIENTED_EDGE ( 'NONE', *, *, #5225, .T. ) ;
#970 = DIRECTION ( 'NONE',  ( -0.000000000000000000, -1.000000000000000000, -0.000000000000000000 ) ) ;
#971 = ORIENTED_EDGE ( 'NONE', *, *, #164, .F. ) ;
#972 = CARTESIAN_POINT ( 'NONE',  ( -47.00000000000001421, 118.0000000000000000, 37.49999999999998579 ) ) ;
#973 = DIRECTION ( 'NONE',  ( -1.000000000000000000, -0.000000000000000000, -0.000000000000000000 ) ) ;
#974 = FACE_OUTER_BOUND ( 'NONE', #10751, .T. ) ;
#975 = EDGE_CURVE ( 'NONE', #12569, #15887, #9043, .T. ) ;
#976 = CARTESIAN_POINT ( 'NONE',  ( 2.066987300000001415, 64.00000000000000000, 45.95000000109246940 ) ) ;
#977 = VECTOR ( 'NONE', #19393, 1000.000000000000000 ) ;
#978 = CARTESIAN_POINT ( 'NONE',  ( -24.00000000000000711, 53.00000000000000711, 14.50000000000000000 ) ) ;
#979 = VECTOR ( 'NONE', #4332, 1000.000000000000000 ) ;
#980 = CARTESIAN_POINT ( 'NONE',  ( 1.145374997815830520, 62.22070308213160672, 44.99999999999998579 ) ) ;
#981 = EDGE_LOOP ( 'NONE', ( #1286, #11849, #18751, #17689 ) ) ;
#982 = VERTEX_POINT ( 'NONE', #15919 ) ;
#983 = CARTESIAN_POINT ( 'NONE',  ( -17.04047135212043784, -30.95583473709190159, 7.107427507916957765 ) ) ;
#984 = CIRCLE ( 'NONE', #14440, 2.041999999999999815 ) ;
#985 = CARTESIAN_POINT ( 'NONE',  ( -32.50000000000002132, -6.000000000000000000, -42.50000000000001421 ) ) ;
#986 = ORIENTED_EDGE ( 'NONE', *, *, #5520, .T. ) ;
#987 = CARTESIAN_POINT ( 'NONE',  ( -14.03132541760400009, -26.95583473709189448, 8.642572492083042235 ) ) ;
#988 = EDGE_CURVE ( 'NONE', #18409, #8629, #826, .T. ) ;
#989 = CARTESIAN_POINT ( 'NONE',  ( -5.799326430397251819, 29.65377616443625541, 56.83055285973284754 ) ) ;
#990 = ORIENTED_EDGE ( 'NONE', *, *, #7649, .F. ) ;
#991 = CARTESIAN_POINT ( 'NONE',  ( -18.04416526290808775, -23.36097942780924441, 36.64257249208304756 ) ) ;
#992 = PLANE ( 'NONE',  #18189 ) ;
#993 = VERTEX_POINT ( 'NONE', #12965 ) ;
#994 = CIRCLE ( 'NONE', #16652, 2.500000000000001776 ) ;
#995 = DIRECTION ( 'NONE',  ( -0.000000000000000000, -0.000000000000000000, -1.000000000000000000 ) ) ;
#996 = VERTEX_POINT ( 'NONE', #17478 ) ;
#997 = CARTESIAN_POINT ( 'NONE',  ( -6.528048594804062965, -42.28611686177728046, 3.000000000000000000 ) ) ;
#998 = DIRECTION ( 'NONE',  ( -1.156482317317871478E-16, 1.000000000000000000, 0.000000000000000000 ) ) ;
#999 = AXIS2_PLACEMENT_3D ( 'NONE', #7203, #19169, #14462 ) ;
#1000 = CARTESIAN_POINT ( 'NONE',  ( 3.999999999999998224, 67.00000000000000000, 34.99999999999999289 ) ) ;
#1001 = EDGE_CURVE ( 'NONE', #15589, #6260, #11589, .T. ) ;
#1002 = CARTESIAN_POINT ( 'NONE',  ( -9.999999999999994671, -24.16482700510257686, 21.32617750791695599 ) ) ;
#1003 = EDGE_CURVE ( 'NONE', #16765, #16368, #9344, .T. ) ;
#1004 = CARTESIAN_POINT ( 'NONE',  ( -2.066987300000001415, 64.00000000000000000, 49.55000000109247082 ) ) ;
#1005 = DIRECTION ( 'NONE',  ( -0.000000000000000000, -1.000000000000000000, -0.000000000000000000 ) ) ;
#1006 = ADVANCED_FACE ( 'NONE', ( #4256 ), #4553, .F. ) ;
#1007 = CARTESIAN_POINT ( 'NONE',  ( -12.35725562635143682, -19.75228648362908501, -0.5488224920830419018 ) ) ;
#1008 = DIRECTION ( 'NONE',  ( 0.000000000000000000, 0.000000000000000000, 1.000000000000000000 ) ) ;
#1009 = ORIENTED_EDGE ( 'NONE', *, *, #16981, .F. ) ;
#1010 = CARTESIAN_POINT ( 'NONE',  ( -21.14459132904239169, -20.64274437364858628, 31.61132249208303691 ) ) ;
#1011 = CARTESIAN_POINT ( 'NONE',  ( -12.64274437364855252, -28.41254052147347053, 37.95117750791695954 ) ) ;
#1012 = CARTESIAN_POINT ( 'NONE',  ( -1.461580736456473906, 65.46158073645646880, 49.45000000109246940 ) ) ;
#1013 = CARTESIAN_POINT ( 'NONE',  ( -9.955834737091903364, -25.17491895705294880, 39.26757249208304046 ) ) ;
#1014 = FACE_OUTER_BOUND ( 'NONE', #6410, .T. ) ;
#1015 = EDGE_LOOP ( 'NONE', ( #19019, #777, #10744, #12366, #12548 ) ) ;
#1016 = CLOSED_SHELL ( 'NONE', ( #2998, #16570, #3537, #10721, #5242, #6217, #13298, #18724, #17316, #1952, #11913, #18660, #732, #7313, #10539, #10222, #3338, #15764, #15018, #3137, #11666, #4956, #6976, #2789, #8547, #1023, #10419, #4151, #13881, #18461, #11109, #4449, #9828, #10820, #2175, #10845, #14410, #10785, #8215, #11618, #5050, #3662, #4463, #9985, #5280, #5699, #11404, #10916, #6266, #18784, #14503, #7001, #3782, #14357 ) ) ;
#1017 = DIRECTION ( 'NONE',  ( -0.000000000000000000, -0.000000000000000000, -1.000000000000000000 ) ) ;
#1018 = CARTESIAN_POINT ( 'NONE',  ( -13.49542703274178379, -19.04416526290806289, 35.98242750791696665 ) ) ;
#1019 = LINE ( 'NONE', #10212, #11710 ) ;
#1020 = CARTESIAN_POINT ( 'NONE',  ( -2.500000000000006661, 65.03553390593272354, 45.25000000218494733 ) ) ;
#1021 = DIRECTION ( 'NONE',  ( -1.000000000000000000, -0.000000000000000000, -0.000000000000000000 ) ) ;
#1022 = CARTESIAN_POINT ( 'NONE',  ( -13.49542703274174116, -28.95583473709188738, 34.89257249208303335 ) ) ;
#1023 = ADVANCED_FACE ( 'NONE', ( #7290, #12355, #16508, #9050, #16406, #10215, #5823 ), #19158, .T. ) ;
#1024 = EDGE_CURVE ( 'NONE', #2345, #11043, #14353, .T. ) ;
#1025 = CARTESIAN_POINT ( 'NONE',  ( 4.592425496802577917E-16, 61.50000000000000000, 48.59999999999999432 ) ) ;
#1026 = FACE_OUTER_BOUND ( 'NONE', #3398, .T. ) ;
#1027 = DIRECTION ( 'NONE',  ( 0.000000000000000000, -0.000000000000000000, 1.000000000000000000 ) ) ;
#1028 = CARTESIAN_POINT ( 'NONE',  ( 1.035533905932738197, 66.50000000000000000, 48.94999999999999574 ) ) ;
#1029 = LINE ( 'NONE', #3587, #8038 ) ;
#1030 = EDGE_LOOP ( 'NONE', ( #12141, #15928, #19063, #7063 ) ) ;
#1031 =( NAMED_UNIT ( * ) PLANE_ANGLE_UNIT ( ) SI_UNIT ( $, .RADIAN. ) );
#1032 = CARTESIAN_POINT ( 'NONE',  ( 2.066987300000001415, 64.00000000000000000, 45.15000000109247225 ) ) ;
#1033 = CARTESIAN_POINT ( 'NONE',  ( -14.83517299489739649, -18.99999999999997868, 4.263677507916958653 ) ) ;
#1034 = PLANE ( 'NONE',  #12270 ) ;
#1035 = CARTESIAN_POINT ( 'NONE',  ( -17.04047135212050890, -17.04416526290807710, 37.51757249208304046 ) ) ;
#1036 = CARTESIAN_POINT ( 'NONE',  ( 2.066987300000002303, 63.14382582708705627, 48.50000000109246656 ) ) ;
#1037 = DIRECTION ( 'NONE',  ( -0.000000000000000000, 1.471414886128461471E-15, 1.000000000000000000 ) ) ;
#1038 = CARTESIAN_POINT ( 'NONE',  ( -2.500000000000001776, 64.00000000000000000, 45.30000000218493739 ) ) ;
#1039 = EDGE_CURVE ( 'NONE', #11212, #11751, #10602, .T. ) ;
#1040 = CARTESIAN_POINT ( 'NONE',  ( 2.066987300000001859, 63.14382582708704916, 45.90000000109247225 ) ) ;
#1041 = DIRECTION ( 'NONE',  ( 0.000000000000000000, 0.000000000000000000, -1.000000000000000000 ) ) ;
#1042 = LINE ( 'NONE', #15761, #17575 ) ;
#1043 = DIRECTION ( 'NONE',  ( 1.000000000000000000, 0.000000000000000000, 0.000000000000000000 ) ) ;
#1044 = CARTESIAN_POINT ( 'NONE',  ( 2.500000000000002220, 62.96446609406726225, 44.85000000218494165 ) ) ;
#1045 = ORIENTED_EDGE ( 'NONE', *, *, #6088, .F. ) ;
#1046 = ORIENTED_EDGE ( 'NONE', *, *, #14507, .T. ) ;
#1047 = CARTESIAN_POINT ( 'NONE',  ( -11.64274437364859693, -17.85540867095757989, 6.673822492083038682 ) ) ;
#1048 = FILL_AREA_STYLE ('',( #3808 ) ) ;
#1049 = VERTEX_POINT ( 'NONE', #13256 ) ;
#1051 = ORIENTED_EDGE ( 'NONE', *, *, #5788, .F. ) ;
#1050 = VERTEX_POINT ( 'NONE', #3071 ) ;
#1052 = CARTESIAN_POINT ( 'NONE',  ( -14.03132541760400009, -26.95583473709189448, 40.14257249208306177 ) ) ;
#1053 = CARTESIAN_POINT ( 'NONE',  ( -18.35725562635144925, -17.85540867095761186, 24.82617750791695599 ) ) ;
#1054 = CARTESIAN_POINT ( 'NONE',  ( -24.00000000000000000, 110.0000000000000000, 30.00000000000000000 ) ) ;
#1055 = CARTESIAN_POINT ( 'NONE',  ( 1.035533905932738197, 66.50000000000000000, 46.65000000218494591 ) ) ;
#1056 = FACE_OUTER_BOUND ( 'NONE', #18608, .T. ) ;
#1057 = VERTEX_POINT ( 'NONE', #14943 ) ;
#1058 = DIRECTION ( 'NONE',  ( 1.000000000000000000, -0.000000000000000000, -0.000000000000000000 ) ) ;
#1059 = EDGE_LOOP ( 'NONE', ( #16999, #10652, #8275, #15172 ) ) ;
#1060 = ADVANCED_FACE ( 'NONE', ( #19255 ), #2675, .F. ) ;
#1061 = DIRECTION ( 'NONE',  ( -0.000000000000000000, 0.7071067811865493491, -0.7071067811865456854 ) ) ;
#1062 = EDGE_LOOP ( 'NONE', ( #3805, #13532, #11853, #1160 ) ) ;
#1063 = DIRECTION ( 'NONE',  ( -1.000000000000000000, -0.000000000000000000, -0.000000000000000000 ) ) ;
#1064 = ADVANCED_FACE ( 'NONE', ( #17779 ), #1535, .T. ) ;
#1065 = LINE ( 'NONE', #19012, #11851 ) ;
#1066 = DIRECTION ( 'NONE',  ( 7.304098846218135653E-17, 0.000000000000000000, -1.000000000000000000 ) ) ;
#1067 = CARTESIAN_POINT ( 'NONE',  ( 3.796994071234847710E-16, 61.93301269999999903, 46.55000000109247082 ) ) ;
#1068 = CARTESIAN_POINT ( 'NONE',  ( -9.575581032440643243E-15, 20.69167388793145079, 57.30832611206850657 ) ) ;
#1069 = DIRECTION ( 'NONE',  ( 0.000000000000000000, 0.000000000000000000, -1.000000000000000000 ) ) ;
#1070 = DIRECTION ( 'NONE',  ( 0.000000000000000000, 0.7071067811865456854, 0.7071067811865494601 ) ) ;
#1071 = ORIENTED_EDGE ( 'NONE', *, *, #17380, .T. ) ;
#1073 = ORIENTED_EDGE ( 'NONE', *, *, #11613, .T. ) ;
#1072 = ORIENTED_EDGE ( 'NONE', *, *, #15999, .T. ) ;
#1074 = CARTESIAN_POINT ( 'NONE',  ( -16.50457296725820555, -28.95583473709189448, 38.60742750791694533 ) ) ;
#1075 = DIRECTION ( 'NONE',  ( 0.000000000000000000, 0.000000000000000000, 1.000000000000000000 ) ) ;
#1076 = ORIENTED_EDGE ( 'NONE', *, *, #9823, .F. ) ;
#1077 = AXIS2_PLACEMENT_3D ( 'NONE', #3070, #4653, #6219 ) ;
#1078 = CARTESIAN_POINT ( 'NONE',  ( -14.83517299489736985, -26.99999999999998579, 3.611322492083043123 ) ) ;
#1079 = CARTESIAN_POINT ( 'NONE',  ( -1.035533905932738863, 61.50000000000000000, 45.34999999999999432 ) ) ;
#1080 = ORIENTED_EDGE ( 'NONE', *, *, #9742, .T. ) ;
#1081 = CARTESIAN_POINT ( 'NONE',  ( -15.63902057219076269, -20.95583473709189448, 9.294927507916961318 ) ) ;
#1082 = CARTESIAN_POINT ( 'NONE',  ( -1.530808498934192803E-16, 66.50000000000000000, 48.99999999999999289 ) ) ;
#1083 = ORIENTED_EDGE ( 'NONE', *, *, #3878, .T. ) ;
#1084 = CARTESIAN_POINT ( 'NONE',  ( -1.530808498934192803E-16, 66.50000000000000000, 46.70000000218494307 ) ) ;
#1085 = ORIENTED_EDGE ( 'NONE', *, *, #13084, .F. ) ;
#1086 = CARTESIAN_POINT ( 'NONE',  ( -14.99999999999999645, 73.00000000000001421, 23.99999999999997868 ) ) ;
#1087 = CYLINDRICAL_SURFACE ( 'NONE', #17377, 1.599999999999997202 ) ;
#1088 = AXIS2_PLACEMENT_3D ( 'NONE', #13661, #7596, #6331 ) ;
#1089 = CARTESIAN_POINT ( 'NONE',  ( -2.500000000000001776, 64.00000000000000000, 47.70000000218494307 ) ) ;
#1090 = CIRCLE ( 'NONE', #16120, 2.999999999999999112 ) ;
#1091 = CARTESIAN_POINT ( 'NONE',  ( -1.767766952966370209, 65.76776695296638309, 48.40000000218494591 ) ) ;
#1092 = EDGE_CURVE ( 'NONE', #2343, #576, #12483, .T. ) ;
#1093 = CARTESIAN_POINT ( 'NONE',  ( -9.999999999999994671, -24.16482700510257686, 26.57617750791695954 ) ) ;
#1094 = CARTESIAN_POINT ( 'NONE',  ( -41.00000000000000711, 53.00000000000000711, 0.5000000000000004441 ) ) ;
#1095 = CARTESIAN_POINT ( 'NONE',  ( -18.78091578003889950, -27.53959229564985378, 7.544927507916956877 ) ) ;
#1096 = PLANE ( 'NONE',  #13026 ) ;
#1097 = ORIENTED_EDGE ( 'NONE', *, *, #3003, .F. ) ;
#1098 = CARTESIAN_POINT ( 'NONE',  ( -14.83517299489735741, -28.99999999999998224, 8.861322492083040459 ) ) ;
#1099 = VECTOR ( 'NONE', #2541, 1000.000000000000000 ) ;
#1100 = CARTESIAN_POINT ( 'NONE',  ( -11.35725562635144925, -18.02023567606020293, -0.5488224920830435671 ) ) ;
#1101 = CONICAL_SURFACE ( 'NONE', #9558, 2.055000000000000160, 0.7853981633974712606 ) ;
#1102 = CARTESIAN_POINT ( 'NONE',  ( -1.461580736456473906, 65.46158073645646880, 47.85000000109246798 ) ) ;
#1103 = CARTESIAN_POINT ( 'NONE',  ( -19.95583473709190514, -25.50457296725822687, 36.20507249208303335 ) ) ;
#1104 = CARTESIAN_POINT ( 'NONE',  ( -1.265664690411616068E-16, 66.06698730000000808, 44.55000000109247082 ) ) ;
#1105 = ORIENTED_EDGE ( 'NONE', *, *, #7076, .F. ) ;
#1106 = EDGE_CURVE ( 'NONE', #3347, #18273, #16111, .T. ) ;
#1107 = CARTESIAN_POINT ( 'NONE',  ( -1.767766952966369765, 62.23223304703363112, 46.20000000218494307 ) ) ;
#1108 = CARTESIAN_POINT ( 'NONE',  ( -11.21908421996108629, -20.46040770435011069, 31.16992750791695599 ) ) ;
#1109 = EDGE_CURVE ( 'NONE', #7321, #12653, #14055, .T. ) ;
#1110 = EDGE_CURVE ( 'NONE', #18251, #11621, #16207, .T. ) ;
#1111 = CARTESIAN_POINT ( 'NONE',  ( 1.844224359752661968, -41.39960408384398249, 3.000000000000000000 ) ) ;
#1112 = DIRECTION ( 'NONE',  ( -1.000000000000000000, 0.000000000000000000, -0.000000000000000000 ) ) ;
#1113 = CARTESIAN_POINT ( 'NONE',  ( -2.500000000000001776, 64.00000000000000000, 49.99999999999999289 ) ) ;
#1114 = CARTESIAN_POINT ( 'NONE',  ( -19.95583473709190514, -25.50457296725823042, 41.45507249208304046 ) ) ;
#1115 = CARTESIAN_POINT ( 'NONE',  ( 1.767766952966369987, 65.76776695296638309, 46.49999999999999289 ) ) ;
#1116 = CARTESIAN_POINT ( 'NONE',  ( -2.066987300000001415, 64.85617417291294373, 49.70000000109247651 ) ) ;
#1117 = VECTOR ( 'NONE', #5853, 1000.000000000000000 ) ;
#1118 = VECTOR ( 'NONE', #7896, 1000.000000000000000 ) ;
#1119 = FACE_OUTER_BOUND ( 'NONE', #12928, .T. ) ;
#1120 = CARTESIAN_POINT ( 'NONE',  ( 2.066987300000001859, 64.85617417291294373, 45.40000000109246514 ) ) ;
#1121 = PLANE ( 'NONE',  #13972 ) ;
#1122 = EDGE_LOOP ( 'NONE', ( #4526, #1404, #11624, #13740, #11083 ) ) ;
#1123 =( NAMED_UNIT ( * ) PLANE_ANGLE_UNIT ( ) SI_UNIT ( $, .RADIAN. ) );
#1124 = CARTESIAN_POINT ( 'NONE',  ( -12.35725562635143682, -19.75228648362908501, 4.701177507916957765 ) ) ;
#1125 = CARTESIAN_POINT ( 'NONE',  ( -10.58745947852649927, -21.64274437364853654, 5.138677507916957765 ) ) ;
#1126 = DIRECTION ( 'NONE',  ( -2.602085213965211135E-16, 1.000000000000000000, 0.000000000000000000 ) ) ;
#1127 = CARTESIAN_POINT ( 'NONE',  ( -20.97976432393974022, -27.64274437364858628, 35.98632249208303335 ) ) ;
#1128 = AXIS2_PLACEMENT_3D ( 'NONE', #9817, #18860, #10100 ) ;
#1129 = ADVANCED_FACE ( 'NONE', ( #7187 ), #13161, .F. ) ;
#1130 = AXIS2_PLACEMENT_3D ( 'NONE', #7594, #13560, #10719 ) ;
#1131 = CARTESIAN_POINT ( 'NONE',  ( 1.461580736456473906, 62.53841926354353120, 47.65000000109247225 ) ) ;
#1132 = CARTESIAN_POINT ( 'NONE',  ( -17.95583473709191580, -23.03132541760400898, 34.66992750791696665 ) ) ;
#1133 = CARTESIAN_POINT ( 'NONE',  ( -19.41254052147348830, -26.35725562635142083, 7.763677507916958653 ) ) ;
#1134 = DIRECTION ( 'NONE',  ( -7.304098846218135653E-17, 0.000000000000000000, 1.000000000000000000 ) ) ;
#1135 = EDGE_CURVE ( 'NONE', #5597, #2911, #5918, .T. ) ;
#1136 = CARTESIAN_POINT ( 'NONE',  ( -2.066987300000001415, 64.00000000000000000, 46.35000000109246798 ) ) ;
#1137 = CARTESIAN_POINT ( 'NONE',  ( -31.74999999999995737, 5.204748896376250699E-16, -4.250000000000000000 ) ) ;
#1138 = DIRECTION ( 'NONE',  ( 0.000000000000000000, 0.000000000000000000, -1.000000000000000000 ) ) ;
#1139 = CARTESIAN_POINT ( 'NONE',  ( 2.066987300000001859, 63.14382582708704916, 47.70000000109246940 ) ) ;
#1140 = CARTESIAN_POINT ( 'NONE',  ( 4.189607678530260948, 26.72836399182260791, 59.40336399182267257 ) ) ;
#1141 = VECTOR ( 'NONE', #9980, 1000.000000000000000 ) ;
#1142 = CIRCLE ( 'NONE', #15856, 0.9999999999999974465 ) ;
#1143 = DIRECTION ( 'NONE',  ( 1.000000000000000000, -0.000000000000000000, -0.000000000000000000 ) ) ;
#1144 = EDGE_LOOP ( 'NONE', ( #5694, #7541, #10250, #5866, #13029, #5265, #13684, #11324 ) ) ;
#1145 = ORIENTED_EDGE ( 'NONE', *, *, #7309, .F. ) ;
#1146 = CARTESIAN_POINT ( 'NONE',  ( -18.35725562635144925, -17.85540867095761186, 40.57617750791695244 ) ) ;
#1147 = ORIENTED_EDGE ( 'NONE', *, *, #4748, .T. ) ;
#1149 = ORIENTED_EDGE ( 'NONE', *, *, #13711, .F. ) ;
#1148 = ORIENTED_EDGE ( 'NONE', *, *, #17670, .T. ) ;
#1150 = EDGE_CURVE ( 'NONE', #262, #14577, #1861, .T. ) ;
#1151 = CARTESIAN_POINT ( 'NONE',  ( -12.04416526290808420, -23.03132541760398766, 38.83007249208304756 ) ) ;
#1152 = CARTESIAN_POINT ( 'NONE',  ( -7.955834737091916686, -22.28918265808470522, 36.85742750791695244 ) ) ;
#1153 = CARTESIAN_POINT ( 'NONE',  ( 21.50000000000001421, 115.0000000000000000, 32.49999999999998579 ) ) ;
#1154 = CARTESIAN_POINT ( 'NONE',  ( 0.8561741729129472844, 61.93301270000000613, 49.00000000109246656 ) ) ;
#1155 = DIRECTION ( 'NONE',  ( 0.000000000000000000, -0.4999999999999991118, 0.8660254037844391517 ) ) ;
#1156 = ORIENTED_EDGE ( 'NONE', *, *, #5431, .F. ) ;
#1157 = CARTESIAN_POINT ( 'NONE',  ( -4.160453206537193083, 26.88344170207934525, 59.60057016663802187 ) ) ;
#1158 = VERTEX_POINT ( 'NONE', #1514 ) ;
#1159 = LINE ( 'NONE', #17905, #8587 ) ;
#1160 = ORIENTED_EDGE ( 'NONE', *, *, #1024, .F. ) ;
#1161 = LINE ( 'NONE', #15875, #6006 ) ;
#1162 = CARTESIAN_POINT ( 'NONE',  ( -43.50000000000000711, 115.0000000000000000, -52.50000000000000711 ) ) ;
#1163 = CARTESIAN_POINT ( 'NONE',  ( -5.800000000000006928, 29.47747564417435484, 56.65425233947093631 ) ) ;
#1164 = CARTESIAN_POINT ( 'NONE',  ( 0.8561741729129460632, 66.06698729999999387, 46.90000000109247225 ) ) ;
#1165 = LINE ( 'NONE', #4210, #17235 ) ;
#1166 = DIRECTION ( 'NONE',  ( 0.000000000000000000, 0.000000000000000000, 1.000000000000000000 ) ) ;
#1167 = DIRECTION ( 'NONE',  ( -0.000000000000000000, -0.000000000000000000, -1.000000000000000000 ) ) ;
#1168 = VERTEX_POINT ( 'NONE', #6026 ) ;
#1170 = ORIENTED_EDGE ( 'NONE', *, *, #17994, .F. ) ;
#1169 = ORIENTED_EDGE ( 'NONE', *, *, #14932, .T. ) ;
#1171 = CARTESIAN_POINT ( 'NONE',  ( -18.35725562635144925, -17.85540867095761186, 3.826177507916956433 ) ) ;
#1172 = DIRECTION ( 'NONE',  ( 5.782411586589357392E-17, -0.000000000000000000, 1.000000000000000000 ) ) ;
#1173 = ORIENTED_EDGE ( 'NONE', *, *, #3972, .F. ) ;
#1174 = CARTESIAN_POINT ( 'NONE',  ( -12.31951028609536536, -25.35725562635139596, 7.986322492083044011 ) ) ;
#1175 = DIRECTION ( 'NONE',  ( 0.7071067811865388020, -0.5000000000000074385, 0.5000000000000046629 ) ) ;
#1176 = ORIENTED_EDGE ( 'NONE', *, *, #1238, .T. ) ;
#1177 = CARTESIAN_POINT ( 'NONE',  ( -12.48433729119798130, -25.64274437364855075, 0.7636775079169598746 ) ) ;
#1178 = CARTESIAN_POINT ( 'NONE',  ( -2.499999999999999112, 65.03553390593273775, 49.15000000000000568 ) ) ;
#1179 = EDGE_LOOP ( 'NONE', ( #8689, #16157, #9561, #9596, #14121, #1902 ) ) ;
#1180 = LINE ( 'NONE', #3749, #310 ) ;
#1181 = EDGE_LOOP ( 'NONE', ( #272, #18537, #17775, #4023 ) ) ;
#1182 = DIRECTION ( 'NONE',  ( 0.000000000000000000, 0.000000000000000000, -1.000000000000000000 ) ) ;
#1183 = PLANE ( 'NONE',  #5177 ) ;
#1184 = CARTESIAN_POINT ( 'NONE',  ( -25.00000000000000000, 53.00000000000000711, -6.000000000000005329 ) ) ;
#1185 = SHAPE_DEFINITION_REPRESENTATION ( #6159, #2502 ) ;
#1186 = DIRECTION ( 'NONE',  ( 1.000000000000000000, 0.000000000000000000, 0.000000000000000000 ) ) ;
#1187 = CARTESIAN_POINT ( 'NONE',  ( -11.46040770435012668, -27.78091578003887463, 32.48242750791695954 ) ) ;
#1188 = FACE_OUTER_BOUND ( 'NONE', #1680, .T. ) ;
#1189 = LINE ( 'NONE', #8840, #18689 ) ;
#1190 = CARTESIAN_POINT ( 'NONE',  ( 0.000000000000000000, 0.000000000000000000, 18.00000000000000000 ) ) ;
#1191 = ORIENTED_EDGE ( 'NONE', *, *, #676, .T. ) ;
#1192 = CARTESIAN_POINT ( 'NONE',  ( -16.71081734191520596, -31.04416526290808065, 40.58007249208304756 ) ) ;
#1193 = CARTESIAN_POINT ( 'NONE',  ( -20.97976432393977575, -20.35725562635143504, 3.388677507916956877 ) ) ;
#1194 = DIRECTION ( 'NONE',  ( -1.000000000000000000, 0.000000000000000000, 0.000000000000000000 ) ) ;
#1195 = EDGE_CURVE ( 'NONE', #4388, #12056, #11985, .T. ) ;
#1196 = ADVANCED_FACE ( 'NONE', ( #5210 ), #3442, .T. ) ;
#1197 = CARTESIAN_POINT ( 'NONE',  ( -11.99999999999999289, -23.83517299489735564, 2.298822492083042235 ) ) ;
#1198 = VECTOR ( 'NONE', #922, 1000.000000000000000 ) ;
#1199 = DIRECTION ( 'NONE',  ( 0.000000000000000000, 0.000000000000000000, 1.000000000000000000 ) ) ;
#1200 = VERTEX_POINT ( 'NONE', #15692 ) ;
#1201 = DIRECTION ( 'NONE',  ( -2.775557561562890858E-16, 0.7071067811865456854, 0.7071067811865493491 ) ) ;
#1202 = DIRECTION ( 'NONE',  ( -0.000000000000000000, -1.000000000000000000, -0.000000000000000000 ) ) ;
#1203 = EDGE_CURVE ( 'NONE', #1873, #18422, #909, .T. ) ;
#1204 = CARTESIAN_POINT ( 'NONE',  ( -24.00000000000000000, 53.00000000000000711, 30.00000000000000000 ) ) ;
#1205 = CARTESIAN_POINT ( 'NONE',  ( -19.95583473709191225, -22.49542703274176603, 39.91992750791695954 ) ) ;
#1206 = DIRECTION ( 'NONE',  ( -1.000000000000000000, -0.000000000000000000, -0.000000000000000000 ) ) ;
#1207 = CARTESIAN_POINT ( 'NONE',  ( -13.82508104294702100, -18.95583473709188382, 32.70507249208304046 ) ) ;
#1208 = CARTESIAN_POINT ( 'NONE',  ( 1.767766952966370653, 62.23223304703363112, 46.29999999999999716 ) ) ;
#1209 = CARTESIAN_POINT ( 'NONE',  ( 2.066987300000001859, 63.14382582708704916, 48.50000000109246656 ) ) ;
#1210 = EDGE_CURVE ( 'NONE', #9690, #15813, #699, .T. ) ;
#1211 = AXIS2_PLACEMENT_3D ( 'NONE', #13801, #15278, #3324 ) ;
#1212 = DIRECTION ( 'NONE',  ( -1.156482317317871478E-16, 1.000000000000000000, 0.000000000000000000 ) ) ;
#1213 = CARTESIAN_POINT ( 'NONE',  ( 2.500000000000002220, 62.96446609406726935, 45.54999999999999716 ) ) ;
#1214 = PLANE ( 'NONE',  #18980 ) ;
#1215 = VECTOR ( 'NONE', #16726, 1000.000000000000000 ) ;
#1216 = EDGE_LOOP ( 'NONE', ( #11012, #8822 ) ) ;
#1217 = ADVANCED_FACE ( 'NONE', ( #5019 ), #1978, .T. ) ;
#1218 = CARTESIAN_POINT ( 'NONE',  ( 0.000000000000000000, 0.000000000000000000, 0.000000000000000000 ) ) ;
#1219 = CARTESIAN_POINT ( 'NONE',  ( -11.46040770435012668, -27.78091578003887463, 0.9824275079169582092 ) ) ;
#1220 = CARTESIAN_POINT ( 'NONE',  ( -9.955834737091912245, -22.82508104294696594, 0.1074275079169582509 ) ) ;
#1221 = DIRECTION ( 'NONE',  ( -0.5773502691896282846, -0.8164965809277242581, 0.000000000000000000 ) ) ;
#1222 = CARTESIAN_POINT ( 'NONE',  ( -17.64274437364858983, -19.75228648362910633, 11.04882249208304046 ) ) ;
#1223 = VECTOR ( 'NONE', #16705, 1000.000000000000000 ) ;
#1224 = CARTESIAN_POINT ( 'NONE',  ( -0.8561741729129465073, 61.93301270000000613, 49.10000000109246088 ) ) ;
#1225 = EDGE_CURVE ( 'NONE', #5958, #13683, #9360, .T. ) ;
#1226 = CARTESIAN_POINT ( 'NONE',  ( -15.96867458239597326, -26.95583473709190159, 28.10742750791695954 ) ) ;
#1227 = CARTESIAN_POINT ( 'NONE',  ( -19.24771351637089367, -21.35725562635142438, 3.388677507916958653 ) ) ;
#1228 = VECTOR ( 'NONE', #16896, 1000.000000000000000 ) ;
#1229 = FACE_OUTER_BOUND ( 'NONE', #13960, .T. ) ;
#1230 = CIRCLE ( 'NONE', #7825, 1.280000000000000027 ) ;
#1231 = CARTESIAN_POINT ( 'NONE',  ( 0.1249999999999895917, 25.46464466094064250, 60.66708332270462734 ) ) ;
#1232 = DIRECTION ( 'NONE',  ( 0.7071067811865414665, -0.5000000000000058842, 0.5000000000000028866 ) ) ;
#1233 = DIRECTION ( 'NONE',  ( -1.000000000000000000, 0.000000000000000000, -0.000000000000000000 ) ) ;
#1234 = CARTESIAN_POINT ( 'NONE',  ( -2.066987300000001415, 64.00000000000000000, 48.95000000109246940 ) ) ;
#1235 = LINE ( 'NONE', #1140, #3481 ) ;
#1236 = VECTOR ( 'NONE', #8624, 1000.000000000000000 ) ;
#1237 = EDGE_CURVE ( 'NONE', #17810, #6948, #2262, .T. ) ;
#1238 = EDGE_CURVE ( 'NONE', #3008, #10469, #14216, .T. ) ;
#1239 = CARTESIAN_POINT ( 'NONE',  ( -15.00000000000000000, -32.00000000000000711, 1.500000000000000000 ) ) ;
#1240 = ORIENTED_EDGE ( 'NONE', *, *, #5077, .T. ) ;
#1241 = EDGE_LOOP ( 'NONE', ( #11948, #10912, #17945, #1283, #1566, #9146, #520, #3733, #14803, #5855, #6245, #19227, #15301, #8219, #16469, #17525, #16503, #381, #18039, #7623, #19032, #7521, #5716, #16047, #880, #13494, #16643, #2727, #18760, #1009, #4004, #5780, #2228, #3499, #10444, #726, #9450, #8717, #10174, #15705, #13406, #9481, #5037, #3504, #6291, #11719, #4592, #1657, #18703, #12860, #1476, #9601, #14968, #5586, #12915, #1586, #15890, #10759, #2179, #173, #10361, #17542, #16573, #15103, #6064, #17514, #2445, #2873, #16154, #689, #364, #9395, #4625, #24, #10077, #11238, #16268, #11151, #19225, #9913, #15765, #10497, #6485, #19212, #5003, #15390, #7620, #10672, #10260, #6196, #7749, #1376, #485, #13117, #18781, #6011, #17055, #9084, #1773, #1677 ) ) ;
#1242 = EDGE_CURVE ( 'NONE', #3513, #7725, #3725, .T. ) ;
#1243 = CARTESIAN_POINT ( 'NONE',  ( -9.020235676060250896, -20.35725562635137820, 7.111322492083040459 ) ) ;
#1244 = AXIS2_PLACEMENT_3D ( 'NONE', #13571, #351, #11909 ) ;
#1245 =( NAMED_UNIT ( * ) SI_UNIT ( $, .STERADIAN. ) SOLID_ANGLE_UNIT ( ) );
#1246 = ORIENTED_EDGE ( 'NONE', *, *, #7374, .T. ) ;
#1248 = ORIENTED_EDGE ( 'NONE', *, *, #14177, .T. ) ;
#1247 = EDGE_LOOP ( 'NONE', ( #7632, #14235, #9399, #2813 ) ) ;
#1249 = CARTESIAN_POINT ( 'NONE',  ( -17.07549068051210739, -21.68318583509881847, 3.607427507916959097 ) ) ;
#1250 = EDGE_CURVE ( 'NONE', #19005, #3857, #12736, .T. ) ;
#1251 = CARTESIAN_POINT ( 'NONE',  ( -18.64274437364860049, -18.02023567606023491, 11.04882249208303868 ) ) ;
#1252 =( BOUNDED_CURVE ( )  B_SPLINE_CURVE ( 2, ( #7047, #18828, #13216, #13113, #2628, #11737, #14599, #7248, #5401 ),
 .UNSPECIFIED., .F., .F. ) 
 B_SPLINE_CURVE_WITH_KNOTS ( ( 3, 2, 2, 2, 3 ),
 ( 0.3571428571428571508, 0.3750000000000000000, 0.3928571428571427937, 0.4107142857142855874, 0.4285714285714284366 ),
 .UNSPECIFIED. ) 
 CURVE ( )  GEOMETRIC_REPRESENTATION_ITEM ( )  RATIONAL_B_SPLINE_CURVE ( ( 1.000000000000000000, 0.9238795325112867385, 1.000000000000000000, 0.9238795325112867385, 1.000000000000000000, 0.9238795325112867385, 1.000000000000000000, 0.9238795325112871826, 0.9999999999999995559 ) ) 
 REPRESENTATION_ITEM ( '' )  );
#1253 = AXIS2_PLACEMENT_3D ( 'NONE', #15002, #13527, #2941 ) ;
#1254 = DIRECTION ( 'NONE',  ( 3.826732013112563602E-16, -1.000000000000000000, 0.000000000000000000 ) ) ;
#1255 = CARTESIAN_POINT ( 'NONE',  ( -1.035533905932738863, 61.50000000000000000, 45.45000000218495018 ) ) ;
#1256 = EDGE_LOOP ( 'NONE', ( #16470, #14104, #2812, #8914 ) ) ;
#1257 = ORIENTED_EDGE ( 'NONE', *, *, #3159, .F. ) ;
#1258 = LINE ( 'NONE', #11829, #15370 ) ;
#1259 = VERTEX_POINT ( 'NONE', #9699 ) ;
#1260 = AXIS2_PLACEMENT_3D ( 'NONE', #5822, #17678, #1112 ) ;
#1261 = ORIENTED_EDGE ( 'NONE', *, *, #15118, .T. ) ;
#1262 = DIRECTION ( 'NONE',  ( -1.000000000000000000, -0.000000000000000000, -0.000000000000000000 ) ) ;
#1263 = DIRECTION ( 'NONE',  ( 0.000000000000000000, -0.7071067811865452413, -0.7071067811865497932 ) ) ;
#1264 = DIRECTION ( 'NONE',  ( -0.000000000000000000, -0.000000000000000000, -1.000000000000000000 ) ) ;
#1265 = AXIS2_PLACEMENT_3D ( 'NONE', #12829, #9974, #15788 ) ;
#1266 = CARTESIAN_POINT ( 'NONE',  ( 2.066987300000002303, 63.14382582708705627, 48.50000000109246656 ) ) ;
#1267 = EDGE_CURVE ( 'NONE', #964, #16382, #6768, .T. ) ;
#1268 = CARTESIAN_POINT ( 'NONE',  ( -0.1250000000000104083, 27.33847763108499507, 59.14680374315354783 ) ) ;
#1269 = DIRECTION ( 'NONE',  ( -0.000000000000000000, -0.000000000000000000, -1.000000000000000000 ) ) ;
#1270 = CIRCLE ( 'NONE', #18792, 2.750000000000000000 ) ;
#1271 = CARTESIAN_POINT ( 'NONE',  ( -41.00000000000000000, 47.00000000000000711, 30.00000000000000000 ) ) ;
#1272 = ORIENTED_EDGE ( 'NONE', *, *, #5680, .F. ) ;
#1274 = EDGE_LOOP ( 'NONE', ( #8686, #17929, #678, #19092 ) ) ;
#1273 = VERTEX_POINT ( 'NONE', #15410 ) ;
#1275 = CARTESIAN_POINT ( 'NONE',  ( -12.64274437364855252, -28.41254052147347053, 37.95117750791695954 ) ) ;
#1276 = DIRECTION ( 'NONE',  ( 0.000000000000000000, 0.000000000000000000, -1.000000000000000000 ) ) ;
#1277 = AXIS2_PLACEMENT_3D ( 'NONE', #7864, #13727, #3147 ) ;
#1278 = ORIENTED_EDGE ( 'NONE', *, *, #6601, .F. ) ;
#1279 = ORIENTED_EDGE ( 'NONE', *, *, #12979, .F. ) ;
#1280 = CARTESIAN_POINT ( 'NONE',  ( -13.64274437364857739, -21.31951028609534760, 1.423822492083042901 ) ) ;
#1281 = VECTOR ( 'NONE', #16758, 1000.000000000000000 ) ;
#1282 = CARTESIAN_POINT ( 'NONE',  ( -25.00000000000000000, 53.00000000000000711, 30.00000000000000000 ) ) ;
#1283 = ORIENTED_EDGE ( 'NONE', *, *, #9412, .T. ) ;
#1284 = CARTESIAN_POINT ( 'NONE',  ( -14.83517299489736985, -26.99999999999998579, 40.36132249208304756 ) ) ;
#1285 = CARTESIAN_POINT ( 'NONE',  ( -2.499999999999992450, 65.03553390593275196, 47.65000000218494591 ) ) ;
#1286 = ORIENTED_EDGE ( 'NONE', *, *, #9886, .T. ) ;
#1287 = VECTOR ( 'NONE', #5413, 1000.000000000000000 ) ;
#1288 = DIRECTION ( 'NONE',  ( 0.000000000000000000, -0.4999999999999992784, 0.8660254037844390407 ) ) ;
#1289 = PRODUCT_DEFINITION_SHAPE ( 'NONE', 'NONE',  #18072 ) ;
#1290 = ORIENTED_EDGE ( 'NONE', *, *, #14321, .F. ) ;
#1291 = CARTESIAN_POINT ( 'NONE',  ( -24.00000000000000711, 53.00000000000000711, 21.00000000000000000 ) ) ;
#1292 = CARTESIAN_POINT ( 'NONE',  ( -2.492551403682614186, 28.10514068711927749, 58.38014068711927251 ) ) ;
#1293 = CARTESIAN_POINT ( 'NONE',  ( -1.530808498934192803E-16, 66.50000000000000000, 44.30000000218494449 ) ) ;
#1294 = VECTOR ( 'NONE', #5042, 1000.000000000000000 ) ;
#1295 = EDGE_CURVE ( 'NONE', #12537, #17031, #12824, .T. ) ;
#1296 = APPLICATION_PROTOCOL_DEFINITION ( 'draft international standard', 'automotive_design', 1998, #8438 ) ;
#1297 = CARTESIAN_POINT ( 'NONE',  ( -2.315774708385926139, 31.50514068711928672, 54.98014068711927393 ) ) ;
#1298 = AXIS2_PLACEMENT_3D ( 'NONE', #590, #15497, #8149 ) ;
#1299 = CARTESIAN_POINT ( 'NONE',  ( -11.46040770435012668, -27.78091578003887463, 27.23242750791694888 ) ) ;
#1300 = CYLINDRICAL_SURFACE ( 'NONE', #11120, 6.000000000000000888 ) ;
#1301 = CARTESIAN_POINT ( 'NONE',  ( -19.95583473709191580, -22.49542703274176603, 3.169927507916957321 ) ) ;
#1302 = AXIS2_PLACEMENT_3D ( 'NONE', #9765, #12794, #1134 ) ;
#1303 = CARTESIAN_POINT ( 'NONE',  ( -15.00000000000000000, -32.50000000000000711, -3.000000000000000000 ) ) ;
#1304 = ORIENTED_EDGE ( 'NONE', *, *, #4606, .F. ) ;
#1305 = CARTESIAN_POINT ( 'NONE',  ( -22.04416526290809486, -22.28918265808477628, 41.89257249208304046 ) ) ;
#1306 = VECTOR ( 'NONE', #7410, 1000.000000000000000 ) ;
#1307 = CARTESIAN_POINT ( 'NONE',  ( -14.83517299489740715, -16.99999999999997868, -0.9863224920830435671 ) ) ;
#1308 = CARTESIAN_POINT ( 'NONE',  ( -1.461580736456473462, 62.53841926354353120, 45.65000000109247225 ) ) ;
#1309 = CARTESIAN_POINT ( 'NONE',  ( -16.35725562635141372, -26.68048971390461332, 4.048822492083043123 ) ) ;
#1310 = VECTOR ( 'NONE', #18785, 1000.000000000000000 ) ;
#1311 = DIRECTION ( 'NONE',  ( -1.000000000000000000, -0.000000000000000000, -0.000000000000000000 ) ) ;
#1312 = ORIENTED_EDGE ( 'NONE', *, *, #15617, .F. ) ;
#1313 = DIRECTION ( 'NONE',  ( -1.000000000000000000, 0.000000000000000000, 0.000000000000000000 ) ) ;
#1314 = ORIENTED_EDGE ( 'NONE', *, *, #13054, .F. ) ;
#1315 = CARTESIAN_POINT ( 'NONE',  ( -17.64274437364855430, -28.24771351637087236, 38.82617750791695954 ) ) ;
#1316 = CARTESIAN_POINT ( 'NONE',  ( 20.00000000000000355, -32.00000000000000711, 1.500000000000000000 ) ) ;
#1317 = DIRECTION ( 'NONE',  ( 0.000000000000000000, 0.000000000000000000, 1.000000000000000000 ) ) ;
#1318 = DIRECTION ( 'NONE',  ( 0.000000000000000000, 0.000000000000000000, 1.000000000000000000 ) ) ;
#1319 = CARTESIAN_POINT ( 'NONE',  ( -16.17491895705296656, -29.04416526290807354, 40.58007249208304046 ) ) ;
#1320 = CARTESIAN_POINT ( 'NONE',  ( -1.767766952966369765, 62.23223304703363112, 47.69999999999999574 ) ) ;
#1321 = CARTESIAN_POINT ( 'NONE',  ( 0.8561741729129471734, 61.93301270000000613, 47.60000000109246798 ) ) ;
#1322 = PLANE ( 'NONE',  #17661 ) ;
#1323 = CARTESIAN_POINT ( 'NONE',  ( -2.500000000000001776, 65.03553390593273775, 45.14999999999999858 ) ) ;
#1324 = DIRECTION ( 'NONE',  ( 0.000000000000000000, 0.000000000000000000, -1.000000000000000000 ) ) ;
#1325 = VECTOR ( 'NONE', #4373, 1000.000000000000114 ) ;
#1326 = ORIENTED_EDGE ( 'NONE', *, *, #6127, .T. ) ;
#1327 = FILL_AREA_STYLE ('',( #8960 ) ) ;
#1328 = CARTESIAN_POINT ( 'NONE',  ( -10.04416526290807710, -25.50457296725819489, 0.5449275079169579872 ) ) ;
#1329 = CARTESIAN_POINT ( 'NONE',  ( -12.64274437364855252, -28.41254052147347053, 16.95117750791695954 ) ) ;
#1330 = CARTESIAN_POINT ( 'NONE',  ( -2.169199425089220146, 64.10592246629431656, 45.00000000000000000 ) ) ;
#1331 = CARTESIAN_POINT ( 'NONE',  ( -14.83517299489735741, -28.99999999999998224, 3.611322492083041347 ) ) ;
#1332 = CARTESIAN_POINT ( 'NONE',  ( 2.066987300000001859, 64.85617417291294373, 46.20000000109247651 ) ) ;
#1333 = CARTESIAN_POINT ( 'NONE',  ( -11.46040770435012668, -27.78091578003887463, 0.9824275079169582092 ) ) ;
#1334 = CARTESIAN_POINT ( 'NONE',  ( -19.99999999999999645, -23.83517299489738051, 2.951177507916958209 ) ) ;
#1335 = DIRECTION ( 'NONE',  ( 0.000000000000000000, 0.000000000000000000, -1.000000000000000000 ) ) ;
#1336 = CARTESIAN_POINT ( 'NONE',  ( -45.00000000000000000, 3.000000000000000000, 54.99999999999998579 ) ) ;
#1337 = DIRECTION ( 'NONE',  ( 1.000000000000000000, -0.000000000000000000, -0.000000000000000000 ) ) ;
#1338 = LINE ( 'NONE', #12006, #372 ) ;
#1339 = B_SPLINE_CURVE_WITH_KNOTS ( 'NONE', 3,
 ( #8067, #10986, #6398, #704 ),
 .UNSPECIFIED., .F., .F.,
 ( 4, 4 ),
 ( 0.000000000000000000, 1.000000000000000000 ),
 .UNSPECIFIED. ) ;
#1340 = DIRECTION ( 'NONE',  ( 0.000000000000000000, -0.7071067811865457964, -0.7071067811865492381 ) ) ;
#1341 = LINE ( 'NONE', #7511, #15382 ) ;
#1342 = ADVANCED_FACE ( 'NONE', ( #6586, #5295, #5122 ), #14307, .F. ) ;
#1343 = CARTESIAN_POINT ( 'NONE',  ( -40.00000000000000711, 110.0000000000000000, 8.000000000000000000 ) ) ;
#1344 = ORIENTED_EDGE ( 'NONE', *, *, #13679, .F. ) ;
#1345 = EDGE_LOOP ( 'NONE', ( #11317, #15399, #5466, #15948 ) ) ;
#1346 = CARTESIAN_POINT ( 'NONE',  ( -15.16482700510264436, -16.99999999999997868, 11.48632249208304046 ) ) ;
#1347 = SHAPE_REPRESENTATION_RELATIONSHIP ( 'NONE' , 'NONE' ,  #15288, #12018 ) ;
#1348 = FACE_OUTER_BOUND ( 'NONE', #929, .T. ) ;
#1350 = VERTEX_POINT ( 'NONE', #499 ) ;
#1349 = ORIENTED_EDGE ( 'NONE', *, *, #2635, .F. ) ;
#1351 = CARTESIAN_POINT ( 'NONE',  ( -14.03132541760401786, -21.04416526290806289, 4.482427507916961318 ) ) ;
#1352 = CARTESIAN_POINT ( 'NONE',  ( -24.00000000000000000, 53.00000000000000711, 30.00000000000000000 ) ) ;
#1353 = CARTESIAN_POINT ( 'NONE',  ( -9.020235676060250896, -20.35725562635137820, 7.111322492083040459 ) ) ;
#1354 = CARTESIAN_POINT ( 'NONE',  ( -2.500000000000001776, 64.00000000000000000, 49.99999999999999289 ) ) ;
#1355 = CARTESIAN_POINT ( 'NONE',  ( 1.767766952966369987, 65.76776695296638309, 45.80000000218493739 ) ) ;
#1356 = ORIENTED_EDGE ( 'NONE', *, *, #9299, .F. ) ;
#1357 = ORIENTED_EDGE ( 'NONE', *, *, #4764, .F. ) ;
#1358 = CARTESIAN_POINT ( 'NONE',  ( 1.035533905932739751, 61.50000000000000000, 47.04999999999999716 ) ) ;
#1359 = CARTESIAN_POINT ( 'NONE',  ( 37.49999999999999289, -6.000000000000000000, 47.49999999999997868 ) ) ;
#1360 = EDGE_CURVE ( 'NONE', #16495, #18191, #17257, .T. ) ;
#1361 = EDGE_CURVE ( 'NONE', #8629, #9506, #8151, .T. ) ;
#1362 = ORIENTED_EDGE ( 'NONE', *, *, #9857, .T. ) ;
#1363 = CARTESIAN_POINT ( 'NONE',  ( 1.035533905932738197, 66.50000000000000000, 45.75000000000000000 ) ) ;
#1364 = CARTESIAN_POINT ( 'NONE',  ( -10.52874183968111765, -22.23000804518926543, 4.401948939463559618E-14 ) ) ;
#1365 = PLANE ( 'NONE',  #2180 ) ;
#1366 = ADVANCED_FACE ( 'NONE', ( #8332 ), #874, .F. ) ;
#1367 = CARTESIAN_POINT ( 'NONE',  ( 3.796994071234847710E-16, 61.93301269999999903, 47.55000000109247082 ) ) ;
#1368 = CARTESIAN_POINT ( 'NONE',  ( -41.00000000000000711, 53.00000000000000711, 21.00000000000000000 ) ) ;
#1369 = LINE ( 'NONE', #11947, #8007 ) ;
#1370 = VERTEX_POINT ( 'NONE', #10978 ) ;
#1372 = VERTEX_POINT ( 'NONE', #16983 ) ;
#1371 = ORIENTED_EDGE ( 'NONE', *, *, #6399, .T. ) ;
#1373 = CARTESIAN_POINT ( 'NONE',  ( -17.64274437364855430, -28.24771351637087236, 38.82617750791695954 ) ) ;
#1374 = CARTESIAN_POINT ( 'NONE',  ( 44.99999999999997158, -1.285879139104706187E-16, 55.00000000000000000 ) ) ;
#1375 = EDGE_LOOP ( 'NONE', ( #3971, #16864, #9192, #16577, #12901 ) ) ;
#1376 = ORIENTED_EDGE ( 'NONE', *, *, #4289, .T. ) ;
#1377 = CARTESIAN_POINT ( 'NONE',  ( -13.64274437364857739, -21.31951028609534760, 6.673822492083044011 ) ) ;
#1378 = CARTESIAN_POINT ( 'NONE',  ( -4.012354697599992193, 26.78000129688593134, 59.70432772728315740 ) ) ;
#1379 = CARTESIAN_POINT ( 'NONE',  ( -32.50000000000001421, -6.000000000000000000, 42.49999999999997868 ) ) ;
#1380 = VERTEX_POINT ( 'NONE', #9607 ) ;
#1381 = CARTESIAN_POINT ( 'NONE',  ( -16.35725562635141372, -26.68048971390461332, 40.79882249208304756 ) ) ;
#1382 = CARTESIAN_POINT ( 'NONE',  ( 12.99999999999999822, 0.000000000000000000, 0.000000000000000000 ) ) ;
#1383 = EDGE_LOOP ( 'NONE', ( #16169, #261 ) ) ;
#1384 = EDGE_CURVE ( 'NONE', #7148, #3017, #15594, .T. ) ;
#1385 = CARTESIAN_POINT ( 'NONE',  ( -25.00000000000000000, 113.0000000000000000, 30.00000000000000000 ) ) ;
#1386 = ORIENTED_EDGE ( 'NONE', *, *, #13706, .F. ) ;
#1387 = CARTESIAN_POINT ( 'NONE',  ( 8.000000000000014211, 60.00000000000000711, 45.00000000000000000 ) ) ;
#1388 = CARTESIAN_POINT ( 'NONE',  ( -4.189607678530257395, 32.40336399182267257, 53.72836399182263278 ) ) ;
#1389 = LINE ( 'NONE', #1492, #17894 ) ;
#1390 = APPLICATION_PROTOCOL_DEFINITION ( 'draft international standard', 'automotive_design', 1998, #1429 ) ;
#1391 = CYLINDRICAL_SURFACE ( 'NONE', #7577, 2.500000000000000444 ) ;
#1392 = LINE ( 'NONE', #12066, #10527 ) ;
#1393 = AXIS2_PLACEMENT_3D ( 'NONE', #337, #13652, #7987 ) ;
#1394 = CARTESIAN_POINT ( 'NONE',  ( -9.955834737091912245, -22.82508104294696594, 0.1074275079169582509 ) ) ;
#1395 = CARTESIAN_POINT ( 'NONE',  ( -0.9999999999999945599, -32.00000000000000000, 4.500000000000000888 ) ) ;
#1396 = ORIENTED_EDGE ( 'NONE', *, *, #6504, .F. ) ;
#1397 = PRODUCT_DEFINITION_CONTEXT ( 'detailed design', #10429, 'design' ) ;
#1398 = CARTESIAN_POINT ( 'NONE',  ( -20.00369391078757886, -29.24501739517668142, 41.01757249208304046 ) ) ;
#1399 = CARTESIAN_POINT ( 'NONE',  ( -19.41254052147348830, -26.35725562635142083, 39.26367750791695954 ) ) ;
#1400 = EDGE_CURVE ( 'NONE', #5597, #13388, #7241, .T. ) ;
#1401 = CARTESIAN_POINT ( 'NONE',  ( 3.796994071234847710E-16, 61.93301269999999903, 45.75000000109247367 ) ) ;
#1402 = CARTESIAN_POINT ( 'NONE',  ( -15.16482700510262482, -20.99999999999997513, 0.9863224920830429010 ) ) ;
#1403 = CARTESIAN_POINT ( 'NONE',  ( -1.485306817036799787, -32.50000000000001421, 3.328446124929187455 ) ) ;
#1404 = ORIENTED_EDGE ( 'NONE', *, *, #7566, .F. ) ;
#1405 = AXIS2_PLACEMENT_3D ( 'NONE', #8749, #5726, #9920 ) ;
#1406 = LINE ( 'NONE', #6021, #14690 ) ;
#1407 = ORIENTED_EDGE ( 'NONE', *, *, #2893, .F. ) ;
#1408 = FACE_OUTER_BOUND ( 'NONE', #2091, .T. ) ;
#1409 = LINE ( 'NONE', #10410, #12032 ) ;
#1410 = LINE ( 'NONE', #4162, #6882 ) ;
#1411 = DIRECTION ( 'NONE',  ( 0.000000000000000000, 0.000000000000000000, 1.000000000000000000 ) ) ;
#1412 = CARTESIAN_POINT ( 'NONE',  ( 0.000000000000000000, -32.00000000000000711, 1.500000000000000000 ) ) ;
#1413 = ADVANCED_FACE ( 'NONE', ( #974 ), #5772, .F. ) ;
#1414 = CARTESIAN_POINT ( 'NONE',  ( 2.500000000000002220, 62.96446609406726935, 46.34999999999999432 ) ) ;
#1415 = CARTESIAN_POINT ( 'NONE',  ( 0.8561741729129460632, 66.06698730000000808, 47.90000000109247225 ) ) ;
#1416 = SURFACE_SIDE_STYLE ('',( #7294 ) ) ;
#1417 = CARTESIAN_POINT ( 'NONE',  ( 4.592425496802577917E-16, 61.50000000000000000, 47.79999999999999716 ) ) ;
#1418 = CARTESIAN_POINT ( 'NONE',  ( -25.00000000000000000, 53.00000000000000711, 1.500000000000001332 ) ) ;
#1419 =( GEOMETRIC_REPRESENTATION_CONTEXT ( 3 ) GLOBAL_UNCERTAINTY_ASSIGNED_CONTEXT ( ( #16497 ) ) GLOBAL_UNIT_ASSIGNED_CONTEXT ( ( #13368, #7102, #10323 ) ) REPRESENTATION_CONTEXT ( 'NONE', 'WORKASPACE' ) );
#1420 = AXIS2_PLACEMENT_3D ( 'NONE', #8834, #4433, #7561 ) ;
#1421 = ORIENTED_EDGE ( 'NONE', *, *, #15282, .F. ) ;
#1422 = CARTESIAN_POINT ( 'NONE',  ( -12.64274437364855252, -28.41254052147347053, 6.451177507916959541 ) ) ;
#1423 = EDGE_CURVE ( 'NONE', #12114, #17652, #17346, .T. ) ;
#1424 = CARTESIAN_POINT ( 'NONE',  ( -18.53959229564986799, -20.21908421996107563, 19.35742750791695599 ) ) ;
#1425 = DIRECTION ( 'NONE',  ( 0.000000000000000000, 0.000000000000000000, -1.000000000000000000 ) ) ;
#1426 = CARTESIAN_POINT ( 'NONE',  ( -12.35725562635140307, -28.24771351637085459, 3.173822492083041347 ) ) ;
#1427 = CARTESIAN_POINT ( 'NONE',  ( -1.265664690411616068E-16, 66.06698730000000808, 46.35000000109246798 ) ) ;
#1428 = CARTESIAN_POINT ( 'NONE',  ( -15.63902057219076269, -20.95583473709189448, 40.79492750791695244 ) ) ;
#1429 = APPLICATION_CONTEXT ( 'automotive_design' ) ;
#1430 = AXIS2_PLACEMENT_3D ( 'NONE', #414, #15121, #12459 ) ;
#1431 = CARTESIAN_POINT ( 'NONE',  ( -15.16482700510259640, -28.99999999999998224, 6.888677507916957765 ) ) ;
#1432 = DIRECTION ( 'NONE',  ( 1.000000000000000000, 0.000000000000000000, -0.000000000000000000 ) ) ;
#1433 = CIRCLE ( 'NONE', #3934, 1.599999999999997202 ) ;
#1434 = LINE ( 'NONE', #17909, #15933 ) ;
#1435 = DIRECTION ( 'NONE',  ( -0.000000000000000000, 0.000000000000000000, 1.000000000000000000 ) ) ;
#1436 = CARTESIAN_POINT ( 'NONE',  ( 2.749999999999979128, 118.0000000000000142, -42.68883962248118991 ) ) ;
#1437 = CARTESIAN_POINT ( 'NONE',  ( -2.066987300000001415, 64.85617417291294373, 45.70000000109248361 ) ) ;
#1438 = DIRECTION ( 'NONE',  ( 2.312964634635742957E-16, -1.000000000000000000, 0.000000000000000000 ) ) ;
#1439 = FACE_OUTER_BOUND ( 'NONE', #11726, .T. ) ;
#1440 = ORIENTED_EDGE ( 'NONE', *, *, #17739, .F. ) ;
#1441 = EDGE_LOOP ( 'NONE', ( #5687, #8862, #2256, #4138 ) ) ;
#1442 = CARTESIAN_POINT ( 'NONE',  ( -13.28918265808478694, -16.95583473709189093, 16.95507249208304046 ) ) ;
#1443 = TOROIDAL_SURFACE ( 'NONE', #2378, 2.700000000000000622, 0.2000000000000000111 ) ;
#1444 = SURFACE_STYLE_USAGE ( .BOTH. , #14872 ) ;
#1445 = VECTOR ( 'NONE', #9654, 1000.000000000000000 ) ;
#1446 = DIRECTION ( 'NONE',  ( 0.000000000000000000, -1.000000000000000000, 0.000000000000000000 ) ) ;
#1448 = ORIENTED_EDGE ( 'NONE', *, *, #11863, .T. ) ;
#1447 = VERTEX_POINT ( 'NONE', #12922 ) ;
#1449 = PRODUCT ( 'socket head cap screw_iso_ISO 4762 M5 x 8 - 8N', 'socket head cap screw_iso_ISO 4762 M5 x 8 - 8N', '', ( #10192 ) ) ;
#1450 = CARTESIAN_POINT ( 'NONE',  ( -15.96867458239597326, -26.95583473709190159, 12.35742750791696132 ) ) ;
#1451 = FACE_OUTER_BOUND ( 'NONE', #7733, .T. ) ;
#1452 = CARTESIAN_POINT ( 'NONE',  ( -9.020235676060250896, -20.35725562635137820, 1.861322492083039126 ) ) ;
#1453 = CARTESIAN_POINT ( 'NONE',  ( 2.066987300000001859, 64.85617417291294373, 48.40000000109247225 ) ) ;
#1454 = CARTESIAN_POINT ( 'NONE',  ( 4.592425496802577917E-16, 61.50000000000000000, 44.70000000218494307 ) ) ;
#1455 = ORIENTED_EDGE ( 'NONE', *, *, #8671, .T. ) ;
#1456 = ORIENTED_EDGE ( 'NONE', *, *, #16499, .T. ) ;
#1457 = EDGE_CURVE ( 'NONE', #4615, #996, #11236, .T. ) ;
#1458 = ADVANCED_FACE ( 'NONE', ( #15877 ), #16253, .F. ) ;
#1459 = CARTESIAN_POINT ( 'NONE',  ( -50.00000000000001421, 118.0000000000000142, 59.99999999999997868 ) ) ;
#1460 = LINE ( 'NONE', #14092, #6627 ) ;
#1461 = ORIENTED_EDGE ( 'NONE', *, *, #6526, .T. ) ;
#1462 = DIRECTION ( 'NONE',  ( 0.000000000000000000, 0.7071067811865494601, -0.7071067811865455743 ) ) ;
#1463 = CARTESIAN_POINT ( 'NONE',  ( 4.101219330881969327, 32.64264068711926825, 53.84264068711931372 ) ) ;
#1464 = ADVANCED_FACE ( 'NONE', ( #18916 ), #11445, .T. ) ;
#1465 = AXIS2_PLACEMENT_3D ( 'NONE', #512, #7971, #1987 ) ;
#1466 = CARTESIAN_POINT ( 'NONE',  ( -2.066987300000001415, 63.14382582708705627, 47.40000000109247225 ) ) ;
#1467 = AXIS2_PLACEMENT_3D ( 'NONE', #4932, #18736, #5216 ) ;
#1468 = LINE ( 'NONE', #18234, #16955 ) ;
#1469 = EDGE_CURVE ( 'NONE', #16449, #6389, #7140, .T. ) ;
#1470 = CARTESIAN_POINT ( 'NONE',  ( -7.999999999999986677, 68.00000000000000000, 66.99999999999997158 ) ) ;
#1471 = EDGE_LOOP ( 'NONE', ( #15796, #4172, #5621, #13747 ) ) ;
#1473 = ORIENTED_EDGE ( 'NONE', *, *, #18638, .T. ) ;
#1472 = ORIENTED_EDGE ( 'NONE', *, *, #6683, .T. ) ;
#1474 = CARTESIAN_POINT ( 'NONE',  ( -11.64274437364854187, -30.14459132904234195, 22.20117750791695599 ) ) ;
#1475 = CARTESIAN_POINT ( 'NONE',  ( -41.00000000000000711, 53.00000000000000711, -24.49999999999999645 ) ) ;
#1476 = ORIENTED_EDGE ( 'NONE', *, *, #15747, .T. ) ;
#1477 = ORIENTED_EDGE ( 'NONE', *, *, #18253, .F. ) ;
#1478 = CARTESIAN_POINT ( 'NONE',  ( -13.35725562635141195, -26.51566270880198672, 13.67382249208304401 ) ) ;
#1479 = EDGE_CURVE ( 'NONE', #4790, #1553, #4307, .T. ) ;
#1480 = CIRCLE ( 'NONE', #3362, 4.000000000000000000 ) ;
#1481 = DIRECTION ( 'NONE',  ( -0.000000000000000000, -1.000000000000000000, -0.000000000000000000 ) ) ;
#1482 = LINE ( 'NONE', #6087, #16267 ) ;
#1483 = ORIENTED_EDGE ( 'NONE', *, *, #18646, .T. ) ;
#1484 = CARTESIAN_POINT ( 'NONE',  ( -17.95583473709191580, -23.03132541760400898, 8.419927507916959541 ) ) ;
#1485 = CARTESIAN_POINT ( 'NONE',  ( -24.00000000000000000, 52.00000000000000711, 30.00000000000000000 ) ) ;
#1486 = ORIENTED_EDGE ( 'NONE', *, *, #7089, .F. ) ;
#1487 = CARTESIAN_POINT ( 'NONE',  ( -37.50000000000002132, 107.3545527679194436, -25.00000000000002132 ) ) ;
#1488 = ORIENTED_EDGE ( 'NONE', *, *, #13083, .F. ) ;
#1489 = ADVANCED_FACE ( 'NONE', ( #19013 ), #19107, .F. ) ;
#1490 = CARTESIAN_POINT ( 'NONE',  ( 21.49999999999997513, 2.999000000000001442, -52.50000000000002132 ) ) ;
#1491 = CARTESIAN_POINT ( 'NONE',  ( -0.1250000000000104083, 25.46464466094064250, 60.66708332270462734 ) ) ;
#1492 = CARTESIAN_POINT ( 'NONE',  ( -24.00000000000000000, 110.0000000000000000, 30.00000000000000000 ) ) ;
#1493 = APPLICATION_PROTOCOL_DEFINITION ( 'draft international standard', 'automotive_design', 1998, #3327 ) ;
#1494 = CARTESIAN_POINT ( 'NONE',  ( -2.499999999999992006, 62.96446609406726225, 46.15000000218496012 ) ) ;
#1495 =( BOUNDED_CURVE ( )  B_SPLINE_CURVE ( 2, ( #13526, #5696, #104, #7154, #11657 ),
 .UNSPECIFIED., .F., .F. ) 
 B_SPLINE_CURVE_WITH_KNOTS ( ( 3, 2, 3 ),
 ( 0.8571428571428569843, 0.8750000000000000000, 0.8928571428571429047 ),
 .UNSPECIFIED. ) 
 CURVE ( )  GEOMETRIC_REPRESENTATION_ITEM ( )  RATIONAL_B_SPLINE_CURVE ( ( 1.000000000000000444, 0.9238795325112862944, 1.000000000000000000, 0.9238795325112867385, 1.000000000000000000 ) ) 
 REPRESENTATION_ITEM ( '' )  );
#1496 = CARTESIAN_POINT ( 'NONE',  ( -20.04416526290808065, -25.17491895705300209, 39.48242750791695244 ) ) ;
#1497 = DIRECTION ( 'NONE',  ( -1.000000000000000000, 0.000000000000000000, 0.000000000000000000 ) ) ;
#1498 = CARTESIAN_POINT ( 'NONE',  ( -9.999999999999994671, -24.16482700510257686, 21.32617750791695599 ) ) ;
#1499 = CARTESIAN_POINT ( 'NONE',  ( 0.000000000000000000, 64.00000000000000000, 49.99999999999999289 ) ) ;
#1500 = EDGE_CURVE ( 'NONE', #6864, #2345, #4009, .T. ) ;
#1501 = ORIENTED_EDGE ( 'NONE', *, *, #15636, .T. ) ;
#1502 = ADVANCED_FACE ( 'NONE', ( #11641 ), #1365, .F. ) ;
#1503 = CARTESIAN_POINT ( 'NONE',  ( -10.58745947852648328, -26.35725562635138530, 7.986322492083041347 ) ) ;
#1504 = CARTESIAN_POINT ( 'NONE',  ( -0.8561741729129461742, 66.06698729999999387, 44.60000000109246088 ) ) ;
#1505 = EDGE_CURVE ( 'NONE', #6482, #5462, #13443, .T. ) ;
#1506 = CARTESIAN_POINT ( 'NONE',  ( -17.51566270880199738, -25.64274437364856496, 9.736322492083042235 ) ) ;
#1507 = CARTESIAN_POINT ( 'NONE',  ( 1.300000000000000044, 1.478016689125442484, -1.626303258728256651E-15 ) ) ;
#1508 = ORIENTED_EDGE ( 'NONE', *, *, #15852, .T. ) ;
#1509 = CARTESIAN_POINT ( 'NONE',  ( -12.94483980383665589, -18.39989183304783538, -8.139499971890162088E-17 ) ) ;
#1510 = ORIENTED_EDGE ( 'NONE', *, *, #3396, .T. ) ;
#1511 = DIRECTION ( 'NONE',  ( -1.000000000000000000, 0.000000000000000000, 0.000000000000000000 ) ) ;
#1512 = LINE ( 'NONE', #15234, #5785 ) ;
#1513 = DIRECTION ( 'NONE',  ( -0.000000000000000000, -0.000000000000000000, -1.000000000000000000 ) ) ;
#1514 = CARTESIAN_POINT ( 'NONE',  ( -15.00000000000001066, -19.99999999999997868, -4.814824860968089633E-32 ) ) ;
#1515 = FACE_OUTER_BOUND ( 'NONE', #9786, .T. ) ;
#1516 = CARTESIAN_POINT ( 'NONE',  ( 0.8561741729129460632, 66.06698730000000808, 45.50000000109247367 ) ) ;
#1517 = ADVANCED_BREP_SHAPE_REPRESENTATION ( '', ( #3741, #1791 ), #13038 ) ;
#1518 = EDGE_CURVE ( 'NONE', #3704, #12114, #13114, .T. ) ;
#1519 = CARTESIAN_POINT ( 'NONE',  ( 1.035533905932738197, 66.50000000000000000, 47.34999999999999432 ) ) ;
#1520 = FACE_OUTER_BOUND ( 'NONE', #6704, .T. ) ;
#1521 = ORIENTED_EDGE ( 'NONE', *, *, #17939, .T. ) ;
#1522 = AXIS2_PLACEMENT_3D ( 'NONE', #18304, #18691, #9555 ) ;
#1523 = FILL_AREA_STYLE_COLOUR ( '', #770 ) ;
#1524 = CARTESIAN_POINT ( 'NONE',  ( -16.50457296725820555, -28.95583473709189448, 7.107427507916955989 ) ) ;
#1525 = CARTESIAN_POINT ( 'NONE',  ( -20.04416526290808065, -25.17491895705300209, 13.23242750791695777 ) ) ;
#1526 = CARTESIAN_POINT ( 'NONE',  ( -1.909647267044692676, 63.20899822134837365, 45.00000000000000000 ) ) ;
#1527 = CARTESIAN_POINT ( 'NONE',  ( -9.955834737091903364, -25.17491895705294880, 7.767572492083041347 ) ) ;
#1528 = CARTESIAN_POINT ( 'NONE',  ( -1.461580736456473906, 65.46158073645646880, 45.65000000109247225 ) ) ;
#1529 = CARTESIAN_POINT ( 'NONE',  ( -17.99999999999999645, -23.83517299489736985, 39.70117750791695954 ) ) ;
#1530 = DIRECTION ( 'NONE',  ( -0.000000000000000000, -0.000000000000000000, -1.000000000000000000 ) ) ;
#1531 = CARTESIAN_POINT ( 'NONE',  ( -13.49542703274178201, -19.04416526290806289, 4.482427507916958653 ) ) ;
#1532 = DIRECTION ( 'NONE',  ( 1.000000000000000000, -0.000000000000000000, -0.000000000000000000 ) ) ;
#1533 = CARTESIAN_POINT ( 'NONE',  ( -2.066987300000001859, 64.85617417291294373, 49.70000000109248361 ) ) ;
#1534 = CARTESIAN_POINT ( 'NONE',  ( -41.00000000000000711, 53.00000000000000711, 8.000000000000000000 ) ) ;
#1535 = TOROIDAL_SURFACE ( 'NONE', #3092, 2.600000000000000089, 0.1499999999999999944 ) ;
#1536 = CARTESIAN_POINT ( 'NONE',  ( -0.9999999999999945599, -28.00000000000000000, 9.500000000000001776 ) ) ;
#1537 = DIRECTION ( 'NONE',  ( -0.000000000000000000, -0.000000000000000000, -1.000000000000000000 ) ) ;
#1538 = CARTESIAN_POINT ( 'NONE',  ( -1.485306817036799787, -37.50000000000000000, 7.999999999999996447 ) ) ;
#1539 = LINE ( 'NONE', #7513, #3636 ) ;
#1540 = ORIENTED_EDGE ( 'NONE', *, *, #6380, .F. ) ;
#1541 = ORIENTED_EDGE ( 'NONE', *, *, #1225, .T. ) ;
#1542 = CARTESIAN_POINT ( 'NONE',  ( -17.04047135212050890, -17.04416526290807710, 21.76757249208304401 ) ) ;
#1543 = CIRCLE ( 'NONE', #1211, 2.750000000000000000 ) ;
#1544 = FILL_AREA_STYLE ('',( #13284 ) ) ;
#1545 = FACE_OUTER_BOUND ( 'NONE', #11575, .T. ) ;
#1547 = ORIENTED_EDGE ( 'NONE', *, *, #16219, .T. ) ;
#1546 = ORIENTED_EDGE ( 'NONE', *, *, #14757, .F. ) ;
#1548 = CARTESIAN_POINT ( 'NONE',  ( -12.04416526290807887, -24.96867458239596260, 11.04492750791696132 ) ) ;
#1549 = CARTESIAN_POINT ( 'NONE',  ( -8.855408670957602979, -27.35725562635137820, 2.736322492083039126 ) ) ;
#1550 = VECTOR ( 'NONE', #9672, 1000.000000000000000 ) ;
#1551 = DIRECTION ( 'NONE',  ( 0.000000000000000000, 0.000000000000000000, -1.000000000000000000 ) ) ;
#1552 = CARTESIAN_POINT ( 'NONE',  ( 0.8561741729129460632, 66.06698729999999387, 49.30000000109246372 ) ) ;
#1553 = VERTEX_POINT ( 'NONE', #5578 ) ;
#1554 = EDGE_LOOP ( 'NONE', ( #9866, #4096, #2330, #1508, #682, #6069 ) ) ;
#1555 = LINE ( 'NONE', #17724, #16314 ) ;
#1556 = ORIENTED_EDGE ( 'NONE', *, *, #2054, .F. ) ;
#1557 = ORIENTED_EDGE ( 'NONE', *, *, #5324, .T. ) ;
#1558 = CARTESIAN_POINT ( 'NONE',  ( 24.00000000000000000, 52.00000000000000711, -50.00000000000000000 ) ) ;
#1559 = CARTESIAN_POINT ( 'NONE',  ( 2.315774708385922587, 27.80336399182260720, 58.32836399182267684 ) ) ;
#1560 = AXIS2_PLACEMENT_3D ( 'NONE', #5311, #3743, #6869 ) ;
#1561 = CARTESIAN_POINT ( 'NONE',  ( -0.8561741729129465073, 61.93301270000000613, 46.70000000109248361 ) ) ;
#1562 = CARTESIAN_POINT ( 'NONE',  ( 4.042620306204053549, 26.80012125920691446, 59.68389060951044200 ) ) ;
#1563 = VECTOR ( 'NONE', #33, 1000.000000000000000 ) ;
#1564 = EDGE_CURVE ( 'NONE', #16934, #16046, #11536, .T. ) ;
#1565 = PLANE ( 'NONE',  #2988 ) ;
#1566 = ORIENTED_EDGE ( 'NONE', *, *, #11894, .F. ) ;
#1568 = ORIENTED_EDGE ( 'NONE', *, *, #12470, .F. ) ;
#1567 = ORIENTED_EDGE ( 'NONE', *, *, #5324, .F. ) ;
#1569 = EDGE_CURVE ( 'NONE', #18409, #6170, #16064, .T. ) ;
#1570 = CARTESIAN_POINT ( 'NONE',  ( -11.64274437364854187, -30.14459132904234195, 11.70117750791695777 ) ) ;
#1571 = PLANE ( 'NONE',  #8360 ) ;
#1572 = VERTEX_POINT ( 'NONE', #2625 ) ;
#1573 = AXIS2_PLACEMENT_3D ( 'NONE', #8509, #17622, #14485 ) ;
#1574 = ORIENTED_EDGE ( 'NONE', *, *, #15403, .F. ) ;
#1575 = CARTESIAN_POINT ( 'NONE',  ( -15.16482700510262482, -20.99999999999997513, 16.73632249208304046 ) ) ;
#1576 = EDGE_CURVE ( 'NONE', #19196, #7027, #4207, .T. ) ;
#1577 = AXIS2_PLACEMENT_3D ( 'NONE', #5121, #15303, #6392 ) ;
#1578 = CARTESIAN_POINT ( 'NONE',  ( 44.99999999999997158, 3.000000000000000000, 53.40000000000000568 ) ) ;
#1579 = PLANE ( 'NONE',  #7195 ) ;
#1580 = ORIENTED_EDGE ( 'NONE', *, *, #12249, .T. ) ;
#1581 = CARTESIAN_POINT ( 'NONE',  ( -14.36097942780923731, -27.04416526290806999, 22.41992750791696309 ) ) ;
#1582 = EDGE_CURVE ( 'NONE', #16384, #14586, #19204, .T. ) ;
#1583 = DIRECTION ( 'NONE',  ( 0.000000000000000000, 0.000000000000000000, 1.000000000000000000 ) ) ;
#1584 = EDGE_LOOP ( 'NONE', ( #18929, #14603 ) ) ;
#1585 = LINE ( 'NONE', #2849, #326 ) ;
#1586 = ORIENTED_EDGE ( 'NONE', *, *, #13525, .T. ) ;
#1587 = LINE ( 'NONE', #4230, #13468 ) ;
#1588 = FACE_OUTER_BOUND ( 'NONE', #481, .T. ) ;
#1589 = LINE ( 'NONE', #114, #9423 ) ;
#1590 = AXIS2_PLACEMENT_3D ( 'NONE', #3065, #4546, #10504 ) ;
#1591 = SHAPE_DEFINITION_REPRESENTATION ( #14745, #3576 ) ;
#1592 = CARTESIAN_POINT ( 'NONE',  ( -0.9999999999999945599, -28.00000000000000000, 9.500000000000001776 ) ) ;
#1593 = AXIS2_PLACEMENT_3D ( 'NONE', #11491, #17887, #16509 ) ;
#1594 = CARTESIAN_POINT ( 'NONE',  ( -18.53959229564986799, -20.21908421996107563, 40.35742750791696665 ) ) ;
#1595 = DIRECTION ( 'NONE',  ( 5.782411586589357392E-17, 0.000000000000000000, 1.000000000000000000 ) ) ;
#1596 = EDGE_CURVE ( 'NONE', #8051, #6389, #5872, .T. ) ;
#1597 = CARTESIAN_POINT ( 'NONE',  ( -13.49542703274178379, -19.04416526290806289, 14.98242750791695777 ) ) ;
#1598 = CIRCLE ( 'NONE', #8768, 6.000000000000003553 ) ;
#1599 = DIRECTION ( 'NONE',  ( -1.000000000000000000, 0.000000000000000000, 0.000000000000000000 ) ) ;
#1600 = EDGE_LOOP ( 'NONE', ( #11359, #14227, #16909, #18115 ) ) ;
#1601 = UNCERTAINTY_MEASURE_WITH_UNIT (LENGTH_MEASURE( 1.000000000000000082E-05 ), #14848, 'distance_accuracy_value', 'NONE');
#1602 = CARTESIAN_POINT ( 'NONE',  ( -16.17491895705296656, -29.04416526290807710, 14.33007249208304046 ) ) ;
#1603 = VECTOR ( 'NONE', #13229, 1000.000000000000000 ) ;
#1604 = CARTESIAN_POINT ( 'NONE',  ( -2.500000000000001776, 64.00000000000000000, 47.70000000218494307 ) ) ;
#1605 = CARTESIAN_POINT ( 'NONE',  ( -12.04416526290808420, -23.03132541760398766, 23.08007249208304401 ) ) ;
#1606 = FACE_OUTER_BOUND ( 'NONE', #17122, .T. ) ;
#1607 = VERTEX_POINT ( 'NONE', #1463 ) ;
#1608 = VECTOR ( 'NONE', #13834, 1000.000000000000000 ) ;
#1609 = FACE_OUTER_BOUND ( 'NONE', #7228, .T. ) ;
#1610 = ORIENTED_EDGE ( 'NONE', *, *, #3289, .F. ) ;
#1611 = DIRECTION ( 'NONE',  ( -1.000000000000000000, 0.000000000000000000, 0.000000000000000000 ) ) ;
#1612 = FACE_OUTER_BOUND ( 'NONE', #16172, .T. ) ;
#1613 = VECTOR ( 'NONE', #1909, 1000.000000000000000 ) ;
#1614 = DIRECTION ( 'NONE',  ( 0.000000000000000000, -0.000000000000000000, -1.000000000000000000 ) ) ;
#1615 = LINE ( 'NONE', #12083, #12230 ) ;
#1616 = ADVANCED_FACE ( 'NONE', ( #10368 ), #17935, .T. ) ;
#1617 = EDGE_CURVE ( 'NONE', #14815, #6260, #14889, .T. ) ;
#1618 = CARTESIAN_POINT ( 'NONE',  ( 1.461580736456473906, 62.53841926354353120, 46.85000000109246798 ) ) ;
#1619 = EDGE_CURVE ( 'NONE', #15030, #5693, #13303, .T. ) ;
#1620 = AXIS2_PLACEMENT_3D ( 'NONE', #4076, #940, #8302 ) ;
#1621 = CARTESIAN_POINT ( 'NONE',  ( -1.530808498934192803E-16, 66.50000000000000000, 48.19999999999999574 ) ) ;
#1622 = CARTESIAN_POINT ( 'NONE',  ( -15.00000000000000000, 50.00000000000000711, 37.00000000000000000 ) ) ;
#1623 = AXIS2_PLACEMENT_3D ( 'NONE', #18592, #13139, #4034 ) ;
#1624 = VERTEX_POINT ( 'NONE', #4506 ) ;
#1625 = STYLED_ITEM ( 'NONE', ( #9316 ), #10426 ) ;
#1626 = CARTESIAN_POINT ( 'NONE',  ( 0.000000000000000000, 3.000000000000000000, 0.000000000000000000 ) ) ;
#1627 = CARTESIAN_POINT ( 'NONE',  ( -15.16482700510259640, -28.99999999999998224, 22.63867750791695954 ) ) ;
#1628 = CARTESIAN_POINT ( 'NONE',  ( -19.95583473709191580, -22.49542703274176603, 13.66992750791695599 ) ) ;
#1629 = CARTESIAN_POINT ( 'NONE',  ( -2.500000000000001776, 65.03553390593273775, 49.25000000218494023 ) ) ;
#1630 = CARTESIAN_POINT ( 'NONE',  ( -10.75228648362912232, -21.35725562635138530, 1.861322492083040903 ) ) ;
#1631 = CARTESIAN_POINT ( 'NONE',  ( -24.00000000000000000, 53.00000000000000711, 30.00000000000000000 ) ) ;
#1632 = EDGE_CURVE ( 'NONE', #10157, #8595, #9199, .T. ) ;
#1633 = CARTESIAN_POINT ( 'NONE',  ( -10.04416526290807710, -25.50457296725819489, 5.794927507916955989 ) ) ;
#1634 = EDGE_CURVE ( 'NONE', #19128, #291, #16456, .T. ) ;
#1635 = FACE_OUTER_BOUND ( 'NONE', #15494, .T. ) ;
#1636 = CARTESIAN_POINT ( 'NONE',  ( -16.17491895705301275, -18.95583473709189448, 14.54492750791695599 ) ) ;
#1637 = DIRECTION ( 'NONE',  ( -1.541976423090495880E-16, 0.000000000000000000, 1.000000000000000000 ) ) ;
#1638 = CARTESIAN_POINT ( 'NONE',  ( 0.8561741729129460632, 66.06698729999999387, 47.90000000109247225 ) ) ;
#1639 = LINE ( 'NONE', #12205, #13397 ) ;
#1640 = AXIS2_PLACEMENT_3D ( 'NONE', #2314, #2693, #1221 ) ;
#1641 = DIRECTION ( 'NONE',  ( -0.000000000000000000, -0.000000000000000000, 1.000000000000000000 ) ) ;
#1642 = CARTESIAN_POINT ( 'NONE',  ( -2.066987300000001415, 64.00000000000000000, 46.55000000109247082 ) ) ;
#1643 = CARTESIAN_POINT ( 'NONE',  ( 7.500000000000005329, -38.00000000000000000, 9.500000000000001776 ) ) ;
#1644 = CARTESIAN_POINT ( 'NONE',  ( 1.300000000000000044, -0.7390083445627200209, 1.280000000000001137 ) ) ;
#1645 = FACE_OUTER_BOUND ( 'NONE', #683, .T. ) ;
#1646 = VERTEX_POINT ( 'NONE', #279 ) ;
#1647 = VERTEX_POINT ( 'NONE', #6265 ) ;
#1648 = CARTESIAN_POINT ( 'NONE',  ( -8.044165262908093084, -21.95952864787946979, 23.08007249208303691 ) ) ;
#1649 = PLANE ( 'NONE',  #18504 ) ;
#1651 = ORIENTED_EDGE ( 'NONE', *, *, #13062, .T. ) ;
#1650 = ORIENTED_EDGE ( 'NONE', *, *, #21, .T. ) ;
#1652 = CARTESIAN_POINT ( 'NONE',  ( -12.31951028609537602, -22.64274437364854364, 15.63867750791696309 ) ) ;
#1653 = LINE ( 'NONE', #1352, #15830 ) ;
#1654 = CARTESIAN_POINT ( 'NONE',  ( -21.99999999999999289, -24.16482700510262305, 4.923822492083038682 ) ) ;
#1655 = CARTESIAN_POINT ( 'NONE',  ( 0.8561741729129460632, 66.06698729999999387, 48.50000000109246656 ) ) ;
#1656 = CARTESIAN_POINT ( 'NONE',  ( 3.796994071234847710E-16, 61.93301269999999903, 48.15000000109247225 ) ) ;
#1657 = ORIENTED_EDGE ( 'NONE', *, *, #14988, .T. ) ;
#1658 = EDGE_CURVE ( 'NONE', #6570, #18891, #1755, .T. ) ;
#1659 = ORIENTED_EDGE ( 'NONE', *, *, #17, .T. ) ;
#1660 = CARTESIAN_POINT ( 'NONE',  ( 1.767766952966369987, 65.76776695296638309, 45.80000000218493739 ) ) ;
#1661 = VERTEX_POINT ( 'NONE', #2925 ) ;
#1662 = VERTEX_POINT ( 'NONE', #12233 ) ;
#1663 = DIRECTION ( 'NONE',  ( -1.000000000000000000, -6.123233995736588542E-17, 0.000000000000000000 ) ) ;
#1664 = FACE_OUTER_BOUND ( 'NONE', #7252, .T. ) ;
#1665 = CARTESIAN_POINT ( 'NONE',  ( 2.066987300000002303, 63.14382582708705627, 46.90000000109247225 ) ) ;
#1666 = DIRECTION ( 'NONE',  ( 0.000000000000000000, 0.000000000000000000, -1.000000000000000000 ) ) ;
#1667 = CARTESIAN_POINT ( 'NONE',  ( -1.767766952966370209, 65.76776695296638309, 47.60000000218494165 ) ) ;
#1668 = ORIENTED_EDGE ( 'NONE', *, *, #14320, .T. ) ;
#1670 = ORIENTED_EDGE ( 'NONE', *, *, #15477, .T. ) ;
#1669 = ORIENTED_EDGE ( 'NONE', *, *, #17624, .T. ) ;
#1671 = CARTESIAN_POINT ( 'NONE',  ( -15.16482700510258574, -30.99999999999998224, 12.13867750791695421 ) ) ;
#1672 = ORIENTED_EDGE ( 'NONE', *, *, #15752, .T. ) ;
#1673 = VERTEX_POINT ( 'NONE', #10756 ) ;
#1674 = CARTESIAN_POINT ( 'NONE',  ( -17.07549068051208963, -26.31681416490115311, 20.01757249208304401 ) ) ;
#1675 = CARTESIAN_POINT ( 'NONE',  ( 2.066987300000001415, 64.85617417291294373, 48.40000000109247225 ) ) ;
#1676 = CYLINDRICAL_SURFACE ( 'NONE', #9076, 1.678500596222258556 ) ;
#1677 = ORIENTED_EDGE ( 'NONE', *, *, #16225, .F. ) ;
#1678 = CARTESIAN_POINT ( 'NONE',  ( -14.36097942780923731, -27.04416526290806999, 17.16992750791696309 ) ) ;
#1679 = DIRECTION ( 'NONE',  ( 1.000000000000000000, -0.000000000000000000, -0.000000000000000000 ) ) ;
#1680 = EDGE_LOOP ( 'NONE', ( #9571, #15611, #5276, #16568 ) ) ;
#1681 = CARTESIAN_POINT ( 'NONE',  ( -15.00000000000001954, -17.99999999999997868, -4.814824860968089633E-32 ) ) ;
#1682 = VERTEX_POINT ( 'NONE', #9102 ) ;
#1683 = FACE_BOUND ( 'NONE', #8959, .T. ) ;
#1684 = FACE_OUTER_BOUND ( 'NONE', #7126, .T. ) ;
#1685 = CARTESIAN_POINT ( 'NONE',  ( -25.00000000000000000, 110.0000000000000000, 30.00000000000000000 ) ) ;
#1686 = DIRECTION ( 'NONE',  ( -0.000000000000000000, 0.000000000000000000, -1.000000000000000000 ) ) ;
#1687 = CARTESIAN_POINT ( 'NONE',  ( -2.500000000000001776, 64.00000000000000000, 46.10000000218494165 ) ) ;
#1688 = CARTESIAN_POINT ( 'NONE',  ( -0.1250000000000104083, 25.46464466094064250, 60.66708332270462734 ) ) ;
#1689 = DIRECTION ( 'NONE',  ( 0.000000000000000000, 0.7071067811865456854, 0.7071067811865494601 ) ) ;
#1690 = CARTESIAN_POINT ( 'NONE',  ( -11.21908421996108629, -20.46040770435011069, 20.66992750791695244 ) ) ;
#1691 = CARTESIAN_POINT ( 'NONE',  ( 14.99999999999998579, 47.00000000000000711, 23.99999999999997158 ) ) ;
#1692 = EDGE_LOOP ( 'NONE', ( #8443, #17446, #17916, #6022 ) ) ;
#1693 = CARTESIAN_POINT ( 'NONE',  ( -17.35725562635140307, -28.41254052147349185, 19.79882249208304046 ) ) ;
#1694 = CARTESIAN_POINT ( 'NONE',  ( 0.000000000000000000, 43.06586399182256741, 43.06586399182279479 ) ) ;
#1695 = CARTESIAN_POINT ( 'NONE',  ( -17.07549068051208963, -26.31681416490115311, 20.01757249208304401 ) ) ;
#1696 = CARTESIAN_POINT ( 'NONE',  ( -41.00000000000000711, 53.00000000000000711, -32.00000000000000000 ) ) ;
#1697 = ORIENTED_EDGE ( 'NONE', *, *, #7811, .T. ) ;
#1698 = CARTESIAN_POINT ( 'NONE',  ( 1.000000000000000222, -28.00000000000000000, 9.500000000000001776 ) ) ;
#1699 = EDGE_LOOP ( 'NONE', ( #18322, #18327, #18029, #18458 ) ) ;
#1700 = LINE ( 'NONE', #15233, #14879 ) ;
#1701 = EDGE_CURVE ( 'NONE', #5403, #7101, #18232, .T. ) ;
#1702 = EDGE_CURVE ( 'NONE', #16934, #9890, #16362, .T. ) ;
#1703 = DIRECTION ( 'NONE',  ( 0.000000000000000000, 0.000000000000000000, -1.000000000000000000 ) ) ;
#1704 = DIRECTION ( 'NONE',  ( -1.000000000000000000, 0.000000000000000000, 0.000000000000000000 ) ) ;
#1705 = VECTOR ( 'NONE', #14150, 1000.000000000000000 ) ;
#1706 = CARTESIAN_POINT ( 'NONE',  ( -1.461580736456473906, 65.46158073645646880, 48.05000000109247082 ) ) ;
#1707 = CYLINDRICAL_SURFACE ( 'NONE', #11087, 2.500000000000000444 ) ;
#1708 = FACE_OUTER_BOUND ( 'NONE', #5051, .T. ) ;
#1709 = CARTESIAN_POINT ( 'NONE',  ( 8.000000000000003553, -25.00000000000000711, 0.000000000000000000 ) ) ;
#1710 = VERTEX_POINT ( 'NONE', #6172 ) ;
#1712 = STYLED_ITEM ( 'NONE', ( #13172 ), #16479 ) ;
#1711 = DIRECTION ( 'NONE',  ( 0.000000000000000000, 0.000000000000000000, 1.000000000000000000 ) ) ;
#1713 = CARTESIAN_POINT ( 'NONE',  ( -19.24771351637089367, -21.35725562635142438, 24.38867750791695954 ) ) ;
#1714 = EDGE_CURVE ( 'NONE', #13315, #14325, #16755, .T. ) ;
#1715 = VECTOR ( 'NONE', #6233, 1000.000000000000000 ) ;
#1716 = CARTESIAN_POINT ( 'NONE',  ( -2.500000000000000888, 62.96446609406726935, 47.75000000218494023 ) ) ;
#1717 = ADVANCED_FACE ( 'NONE', ( #1664 ), #14985, .T. ) ;
#1718 = CARTESIAN_POINT ( 'NONE',  ( -12.64274437364858628, -19.58745947852646552, 22.42382249208304401 ) ) ;
#1719 = EDGE_CURVE ( 'NONE', #7260, #9088, #15187, .T. ) ;
#1720 = CARTESIAN_POINT ( 'NONE',  ( -2.066987300000001415, 64.00000000000000000, 44.95000000109246940 ) ) ;
#1721 = CARTESIAN_POINT ( 'NONE',  ( -19.24771351637089367, -21.35725562635142438, 3.388677507916958653 ) ) ;
#1722 = DIRECTION ( 'NONE',  ( 1.000000000000000000, 0.000000000000000000, 2.081668171172167774E-16 ) ) ;
#1723 = CARTESIAN_POINT ( 'NONE',  ( -16.50457296725820555, -28.95583473709189803, 22.85742750791695954 ) ) ;
#1724 = DIRECTION ( 'NONE',  ( 0.7071067811865513475, 0.4999999999999988898, -0.4999999999999959477 ) ) ;
#1725 = DIRECTION ( 'NONE',  ( 0.000000000000000000, -1.000000000000000000, 0.000000000000000000 ) ) ;
#1726 = CARTESIAN_POINT ( 'NONE',  ( -1.265664690411616068E-16, 66.06698730000000808, 48.75000000109246656 ) ) ;
#1727 = DIRECTION ( 'NONE',  ( 0.000000000000000000, 0.000000000000000000, 1.000000000000000000 ) ) ;
#1728 = EDGE_LOOP ( 'NONE', ( #18520, #15861, #6751, #2742 ) ) ;
#1729 = CARTESIAN_POINT ( 'NONE',  ( 14.99999999999998579, 73.00000000000001421, 23.99999999999997158 ) ) ;
#1730 = AXIS2_PLACEMENT_3D ( 'NONE', #1783, #3543, #6587 ) ;
#1731 = CARTESIAN_POINT ( 'NONE',  ( 0.8561741729129471734, 61.93301270000000613, 46.00000000109246656 ) ) ;
#1732 = CARTESIAN_POINT ( 'NONE',  ( -0.8561741729129465073, 61.93301270000000613, 46.70000000109248361 ) ) ;
#1733 = DIRECTION ( 'NONE',  ( -0.7071067811865463515, 0.000000000000000000, -0.7071067811865487940 ) ) ;
#1734 = DIRECTION ( 'NONE',  ( 1.000000000000000000, -0.000000000000000000, -0.000000000000000000 ) ) ;
#1735 = ORIENTED_EDGE ( 'NONE', *, *, #7505, .F. ) ;
#1736 = VERTEX_POINT ( 'NONE', #11943 ) ;
#1737 = CARTESIAN_POINT ( 'NONE',  ( -20.97976432393974022, -27.64274437364858628, 20.23632249208303691 ) ) ;
#1738 = EDGE_CURVE ( 'NONE', #5670, #2431, #7535, .T. ) ;
#1739 = CARTESIAN_POINT ( 'NONE',  ( -9.999999999999994671, -23.83517299489734143, 18.04882249208304401 ) ) ;
#1741 = VERTEX_POINT ( 'NONE', #18031 ) ;
#1740 = ORIENTED_EDGE ( 'NONE', *, *, #6968, .F. ) ;
#1742 = CARTESIAN_POINT ( 'NONE',  ( -17.07549068051210739, -21.68318583509881847, 19.35742750791695954 ) ) ;
#1743 = DIRECTION ( 'NONE',  ( 0.000000000000000000, -1.000000000000000000, 0.000000000000000000 ) ) ;
#1744 = CARTESIAN_POINT ( 'NONE',  ( -22.04416526290809486, -22.28918265808477628, 26.14257249208303691 ) ) ;
#1745 = TOROIDAL_SURFACE ( 'NONE', #5211, 4.000000000000000000, 0.2500000000000000000 ) ;
#1746 = CARTESIAN_POINT ( 'NONE',  ( 2.066987300000002303, 63.14382582708705627, 48.30000000109247082 ) ) ;
#1747 = CARTESIAN_POINT ( 'NONE',  ( 1.461580736456473684, 65.46158073645646880, 46.85000000109246798 ) ) ;
#1748 = ORIENTED_EDGE ( 'NONE', *, *, #13669, .T. ) ;
#1749 = ORIENTED_EDGE ( 'NONE', *, *, #8582, .T. ) ;
#1750 = ADVANCED_FACE ( 'NONE', ( #4605 ), #13604, .T. ) ;
#1751 = DIRECTION ( 'NONE',  ( 0.000000000000000000, 0.000000000000000000, 1.000000000000000000 ) ) ;
#1752 = DIRECTION ( 'NONE',  ( -0.000000000000000000, -0.000000000000000000, -1.000000000000000000 ) ) ;
#1753 = ORIENTED_EDGE ( 'NONE', *, *, #9630, .F. ) ;
#1754 = FACE_OUTER_BOUND ( 'NONE', #4883, .T. ) ;
#1755 = LINE ( 'NONE', #19303, #8738 ) ;
#1756 = CARTESIAN_POINT ( 'NONE',  ( -25.00000000000000000, 110.0000000000000000, 27.50000000000000000 ) ) ;
#1757 = DIRECTION ( 'NONE',  ( -1.000000000000000000, 0.000000000000000000, 0.000000000000000000 ) ) ;
#1758 = CIRCLE ( 'NONE', #5827, 1.500000000000000222 ) ;
#1759 = VECTOR ( 'NONE', #10320, 1000.000000000000000 ) ;
#1760 = LINE ( 'NONE', #6371, #17711 ) ;
#1761 = EDGE_CURVE ( 'NONE', #16018, #13407, #187, .T. ) ;
#1762 = ORIENTED_EDGE ( 'NONE', *, *, #6968, .T. ) ;
#1764 = ORIENTED_EDGE ( 'NONE', *, *, #10465, .T. ) ;
#1763 = ORIENTED_EDGE ( 'NONE', *, *, #9342, .F. ) ;
#1765 = CARTESIAN_POINT ( 'NONE',  ( -18.64274437364853654, -29.97976432393976509, 17.82617750791695954 ) ) ;
#1766 =( NAMED_UNIT ( * ) PLANE_ANGLE_UNIT ( ) SI_UNIT ( $, .RADIAN. ) );
#1767 = VERTEX_POINT ( 'NONE', #9576 ) ;
#1768 = ORIENTED_EDGE ( 'NONE', *, *, #5180, .F. ) ;
#1769 = CARTESIAN_POINT ( 'NONE',  ( -12.04416526290808420, -23.03132541760398766, 17.83007249208304046 ) ) ;
#1770 = CARTESIAN_POINT ( 'NONE',  ( -9.996306089212364299, -29.24501739517662813, 0.9824275079169565439 ) ) ;
#1771 = CARTESIAN_POINT ( 'NONE',  ( 0.8561741729129460632, 66.06698730000000808, 48.50000000109246656 ) ) ;
#1772 = FACE_OUTER_BOUND ( 'NONE', #8326, .T. ) ;
#1773 = ORIENTED_EDGE ( 'NONE', *, *, #13926, .T. ) ;
#1774 = CARTESIAN_POINT ( 'NONE',  ( -16.64274437364856496, -26.51566270880199738, 23.07617750791695954 ) ) ;
#1775 = VECTOR ( 'NONE', #7172, 1000.000000000000000 ) ;
#1776 = FACE_OUTER_BOUND ( 'NONE', #7352, .T. ) ;
#1777 = ORIENTED_EDGE ( 'NONE', *, *, #12853, .F. ) ;
#1778 = VECTOR ( 'NONE', #16337, 1000.000000000000114 ) ;
#1779 = DIRECTION ( 'NONE',  ( -1.000000000000000000, 0.000000000000000000, 0.000000000000000000 ) ) ;
#1780 = ORIENTED_EDGE ( 'NONE', *, *, #14871, .T. ) ;
#1781 = DIRECTION ( 'NONE',  ( 0.000000000000000000, -1.000000000000000000, 0.000000000000000000 ) ) ;
#1782 = FACE_BOUND ( 'NONE', #2548, .T. ) ;
#1783 = CARTESIAN_POINT ( 'NONE',  ( -43.50000000000000711, 2.999000000000001442, -52.50000000000000711 ) ) ;
#1784 = LINE ( 'NONE', #13730, #2855 ) ;
#1785 = DIRECTION ( 'NONE',  ( 0.000000000000000000, -1.000000000000000000, -0.000000000000000000 ) ) ;
#1786 = LINE ( 'NONE', #16, #13514 ) ;
#1787 = CARTESIAN_POINT ( 'NONE',  ( -2.500000000000001776, 64.00000000000000000, 48.39999999999999858 ) ) ;
#1788 = CARTESIAN_POINT ( 'NONE',  ( -37.50000000000002132, -6.000000000000000000, 47.49999999999997868 ) ) ;
#1789 = VERTEX_POINT ( 'NONE', #4898 ) ;
#1790 = CARTESIAN_POINT ( 'NONE',  ( -14.83517299489739649, -18.99999999999997868, 14.76367750791695777 ) ) ;
#1791 = AXIS2_PLACEMENT_3D ( 'NONE', #13713, #4815, #7646 ) ;
#1792 = DIRECTION ( 'NONE',  ( -0.000000000000000000, -1.000000000000000000, -0.000000000000000000 ) ) ;
#1793 = VERTEX_POINT ( 'NONE', #3414 ) ;
#1794 = UNCERTAINTY_MEASURE_WITH_UNIT (LENGTH_MEASURE( 1.000000000000000082E-05 ), #15170, 'distance_accuracy_value', 'NONE');
#1795 = CARTESIAN_POINT ( 'NONE',  ( -19.24771351637086880, -26.64274437364857206, 14.98632249208304046 ) ) ;
#1796 = CARTESIAN_POINT ( 'NONE',  ( -12.92450931948790149, -21.68318583509881137, 17.39257249208304046 ) ) ;
#1797 = DIRECTION ( 'NONE',  ( 1.000000000000000000, -0.000000000000000000, -0.000000000000000000 ) ) ;
#1798 = VERTEX_POINT ( 'NONE', #15472 ) ;
#1799 = DIRECTION ( 'NONE',  ( 0.000000000000000000, 0.000000000000000000, -1.000000000000000000 ) ) ;
#1800 = EDGE_LOOP ( 'NONE', ( #4603, #7930, #11547 ) ) ;
#1801 = LINE ( 'NONE', #3561, #9692 ) ;
#1802 = CARTESIAN_POINT ( 'NONE',  ( -7.999999999999996447, 0.000000000000000000, 1.500000000000000000 ) ) ;
#1803 = MECHANICAL_DESIGN_GEOMETRIC_PRESENTATION_REPRESENTATION (  '', ( #7753 ), #12112 ) ;
#1804 = CARTESIAN_POINT ( 'NONE',  ( -41.00000000000000711, 53.00000000000000711, -6.000000000000001776 ) ) ;
#1805 = CARTESIAN_POINT ( 'NONE',  ( -40.00000000000000000, 53.00000000000000711, 30.00000000000000000 ) ) ;
#1806 = CARTESIAN_POINT ( 'NONE',  ( 0.000000000000000000, 47.00000000000000711, -50.00000000000000000 ) ) ;
#1807 = CARTESIAN_POINT ( 'NONE',  ( 7.500000000000005329, -26.00000000000000000, 12.50000000000000000 ) ) ;
#1808 = CARTESIAN_POINT ( 'NONE',  ( 14.99999999999998579, 73.00000000000001421, 26.99999999999997158 ) ) ;
#1809 = VERTEX_POINT ( 'NONE', #18426 ) ;
#1810 = B_SPLINE_CURVE_WITH_KNOTS ( 'NONE', 3,
 ( #6841, #15227, #8048, #2057 ),
 .UNSPECIFIED., .F., .F.,
 ( 4, 4 ),
 ( 0.000000000000000000, 1.000000000000000000 ),
 .UNSPECIFIED. ) ;
#1811 = EDGE_CURVE ( 'NONE', #10346, #18257, #10858, .T. ) ;
#1812 = EDGE_CURVE ( 'NONE', #17726, #12801, #3518, .T. ) ;
#1813 = DIRECTION ( 'NONE',  ( 1.000000000000000000, 0.000000000000000000, 0.000000000000000000 ) ) ;
#1814 = CARTESIAN_POINT ( 'NONE',  ( -12.64274437364855252, -28.41254052147347053, 11.70117750791695777 ) ) ;
#1815 = CARTESIAN_POINT ( 'NONE',  ( -2.500000000000000888, 62.96446609406726935, 46.15000000218493881 ) ) ;
#1816 = EDGE_CURVE ( 'NONE', #6405, #8644, #12331, .T. ) ;
#1817 = CARTESIAN_POINT ( 'NONE',  ( -11.46040770435014977, -20.21908421996103655, 17.39257249208304401 ) ) ;
#1818 = DIRECTION ( 'NONE',  ( 0.000000000000000000, 0.4999999999999993894, -0.8660254037844389297 ) ) ;
#1819 = CARTESIAN_POINT ( 'NONE',  ( -15.16482700510259640, -28.99999999999998224, 22.63867750791695954 ) ) ;
#1820 = EDGE_CURVE ( 'NONE', #6791, #1960, #10951, .T. ) ;
#1821 = CARTESIAN_POINT ( 'NONE',  ( -10.00000000000000000, -32.00000000000000711, -3.000000000000000000 ) ) ;
#1822 = CARTESIAN_POINT ( 'NONE',  ( -12.64274437364855252, -28.41254052147347053, 16.95117750791695954 ) ) ;
#1823 = DIRECTION ( 'NONE',  ( -0.5773502691896228445, 0.8164965809277280329, 0.000000000000000000 ) ) ;
#1824 = CARTESIAN_POINT ( 'NONE',  ( -2.500000000000001776, 64.00000000000000000, 46.00000000000000000 ) ) ;
#1825 = CARTESIAN_POINT ( 'NONE',  ( 2.066987300000001415, 64.00000000000000000, 49.35000000109246798 ) ) ;
#1826 = CARTESIAN_POINT ( 'NONE',  ( 9.339266095310328808, -43.78611686177728046, 3.000000000000000000 ) ) ;
#1827 = DIRECTION ( 'NONE',  ( -0.000000000000000000, -0.000000000000000000, -1.000000000000000000 ) ) ;
#1828 = CARTESIAN_POINT ( 'NONE',  ( -1.530808498934192803E-16, 66.50000000000000000, 48.30000000218494449 ) ) ;
#1829 = CARTESIAN_POINT ( 'NONE',  ( 3.796994071234847710E-16, 61.93301269999999903, 49.15000000109246514 ) ) ;
#1830 = DIRECTION ( 'NONE',  ( -0.7071067811865437980, 0.5000000000000039968, -0.5000000000000013323 ) ) ;
#1831 = CIRCLE ( 'NONE', #3394, 1.599999999999997202 ) ;
#1832 = VERTEX_POINT ( 'NONE', #6368 ) ;
#1833 = ORIENTED_EDGE ( 'NONE', *, *, #14412, .F. ) ;
#1834 = CARTESIAN_POINT ( 'NONE',  ( -20.97976432393974022, -27.64274437364858628, 25.48632249208304401 ) ) ;
#1835 = CARTESIAN_POINT ( 'NONE',  ( -14.83517299489735741, -28.99999999999998224, 14.11132249208304046 ) ) ;
#1836 = VERTEX_POINT ( 'NONE', #15760 ) ;
#1837 = CARTESIAN_POINT ( 'NONE',  ( -17.68048971390461688, -25.35725562635141372, 13.01367750791696132 ) ) ;
#1838 = DIRECTION ( 'NONE',  ( 0.000000000000000000, 0.000000000000000000, -1.000000000000000000 ) ) ;
#1839 = CARTESIAN_POINT ( 'NONE',  ( -16.71081734191520596, -31.04416526290808065, 14.33007249208304046 ) ) ;
#1840 = CARTESIAN_POINT ( 'NONE',  ( 0.8561741729129472844, 61.93301270000000613, 48.20000000109248361 ) ) ;
#1841 = CARTESIAN_POINT ( 'NONE',  ( -2.066987300000001859, 64.85617417291294373, 46.30000000109247082 ) ) ;
#1842 = ORIENTED_EDGE ( 'NONE', *, *, #1110, .T. ) ;
#1843 = EDGE_LOOP ( 'NONE', ( #18532, #6957, #6275, #1278 ) ) ;
#1844 = DIRECTION ( 'NONE',  ( 0.000000000000000000, 0.000000000000000000, -1.000000000000000000 ) ) ;
#1845 = LINE ( 'NONE', #7831, #7893 ) ;
#1846 = EDGE_LOOP ( 'NONE', ( #6833, #19010 ) ) ;
#1847 = CARTESIAN_POINT ( 'NONE',  ( -2.283493650000001818, 64.00000000000000000, 49.42500000163870766 ) ) ;
#1848 = DIRECTION ( 'NONE',  ( -0.000000000000000000, -1.000000000000000000, -0.000000000000000000 ) ) ;
#1849 = CARTESIAN_POINT ( 'NONE',  ( -8.528048594804062077, -45.28611686177728046, 1.500000000000000000 ) ) ;
#1850 = EDGE_CURVE ( 'NONE', #8256, #18922, #16853, .T. ) ;
#1851 = ADVANCED_FACE ( 'NONE', ( #15380 ), #1951, .T. ) ;
#1852 = CARTESIAN_POINT ( 'NONE',  ( -1.040834085586084257E-14, 27.62132034355962773, 54.62132034355965260 ) ) ;
#1853 = EDGE_CURVE ( 'NONE', #14031, #2469, #13897, .T. ) ;
#1854 = AXIS2_PLACEMENT_3D ( 'NONE', #6851, #17256, #7042 ) ;
#1855 = CARTESIAN_POINT ( 'NONE',  ( -1.035533905932738863, 61.50000000000000000, 45.45000000218494307 ) ) ;
#1856 = ORIENTED_EDGE ( 'NONE', *, *, #12110, .T. ) ;
#1858 = ORIENTED_EDGE ( 'NONE', *, *, #3600, .F. ) ;
#1857 = EDGE_LOOP ( 'NONE', ( #12020, #9397, #15224, #9214 ) ) ;
#1859 = EDGE_CURVE ( 'NONE', #18257, #10184, #2041, .T. ) ;
#1860 = CARTESIAN_POINT ( 'NONE',  ( -7.999999999999996447, -24.16482700510256976, 37.07617750791694533 ) ) ;
#1861 = CIRCLE ( 'NONE', #4364, 0.1499999999999999667 ) ;
#1862 =( NAMED_UNIT ( * ) SI_UNIT ( $, .STERADIAN. ) SOLID_ANGLE_UNIT ( ) );
#1863 = EDGE_LOOP ( 'NONE', ( #16180, #8342, #18695, #6665 ) ) ;
#1864 = ORIENTED_EDGE ( 'NONE', *, *, #15200, .T. ) ;
#1865 = CARTESIAN_POINT ( 'NONE',  ( -17.51566270880199738, -25.64274437364856496, 14.98632249208304046 ) ) ;
#1866 = CARTESIAN_POINT ( 'NONE',  ( -20.97976432393977575, -20.35725562635143504, 19.13867750791695954 ) ) ;
#1867 = CARTESIAN_POINT ( 'NONE',  ( 0.8561741729129471734, 61.93301270000000613, 47.40000000109247225 ) ) ;
#1868 = DIRECTION ( 'NONE',  ( -1.000000000000000000, 0.000000000000000000, 0.000000000000000000 ) ) ;
#1869 = EDGE_LOOP ( 'NONE', ( #14388, #8355 ) ) ;
#1870 = CARTESIAN_POINT ( 'NONE',  ( -11.95583473709191047, -23.36097942780921954, 21.10742750791696309 ) ) ;
#1871 = CONICAL_SURFACE ( 'NONE', #2791, 2.041999999999999815, 1.047197551196591858 ) ;
#1872 = PRESENTATION_STYLE_ASSIGNMENT (( #300 ) ) ;
#1873 = VERTEX_POINT ( 'NONE', #16954 ) ;
#1874 = VERTEX_POINT ( 'NONE', #18525 ) ;
#1875 = SURFACE_STYLE_FILL_AREA ( #16684 ) ;
#1876 = EDGE_CURVE ( 'NONE', #13296, #19221, #8123, .T. ) ;
#1877 = CARTESIAN_POINT ( 'NONE',  ( -40.00000000000000711, 53.00000000000000711, 8.000000000000000000 ) ) ;
#1878 = EDGE_CURVE ( 'NONE', #1057, #15240, #18707, .T. ) ;
#1879 = PLANE ( 'NONE',  #1577 ) ;
#1880 = FACE_BOUND ( 'NONE', #1843, .T. ) ;
#1881 = VECTOR ( 'NONE', #2671, 1000.000000000000000 ) ;
#1882 = LINE ( 'NONE', #15501, #12863 ) ;
#1883 = CONTEXT_DEPENDENT_SHAPE_REPRESENTATION ( #18730, #11928 ) ;
#1884 = AXIS2_PLACEMENT_3D ( 'NONE', #13511, #17830, #3325 ) ;
#1885 = FACE_OUTER_BOUND ( 'NONE', #13424, .T. ) ;
#1886 = CARTESIAN_POINT ( 'NONE',  ( 0.000000000000000000, 64.00000000000000000, 49.99999999999999289 ) ) ;
#1887 = CARTESIAN_POINT ( 'NONE',  ( 1.035533905932738197, 66.50000000000000000, 49.74999999999998579 ) ) ;
#1888 = CIRCLE ( 'NONE', #9998, 7.000000000000001776 ) ;
#1889 = CARTESIAN_POINT ( 'NONE',  ( 3.678949249685231848, 1.601138781673192758E-19, 0.000000000000000000 ) ) ;
#1890 = ORIENTED_EDGE ( 'NONE', *, *, #760, .F. ) ;
#1891 = CARTESIAN_POINT ( 'NONE',  ( -15.16482700510259640, -28.99999999999998224, 22.63867750791695954 ) ) ;
#1892 = DIRECTION ( 'NONE',  ( 1.000000000000000000, 0.000000000000000000, 0.000000000000000000 ) ) ;
#1893 = ORIENTED_EDGE ( 'NONE', *, *, #12356, .T. ) ;
#1894 = CARTESIAN_POINT ( 'NONE',  ( -13.82508104294702100, -18.95583473709188382, 22.20507249208304401 ) ) ;
#1895 = AXIS2_PLACEMENT_3D ( 'NONE', #17069, #13828, #6484 ) ;
#1896 = CARTESIAN_POINT ( 'NONE',  ( -17.95583473709190869, -24.96867458239598037, 15.20507249208304579 ) ) ;
#1897 =( BOUNDED_CURVE ( )  B_SPLINE_CURVE ( 2, ( #3126, #18429, #1667, #13901, #3522, #10664, #16664, #3229, #388 ),
 .UNSPECIFIED., .F., .F. ) 
 B_SPLINE_CURVE_WITH_KNOTS ( ( 3, 2, 2, 2, 3 ),
 ( 0.2857142857142859205, 0.3035714285714287142, 0.3214285714285715634, 0.3392857142857143571, 0.3571428571428571508 ),
 .UNSPECIFIED. ) 
 CURVE ( )  GEOMETRIC_REPRESENTATION_ITEM ( )  RATIONAL_B_SPLINE_CURVE ( ( 0.9999999999999990008, 0.9238795325112877377, 1.000000000000000000, 0.9238795325112867385, 1.000000000000000000, 0.9238795325112867385, 1.000000000000000000, 0.9238795325112867385, 1.000000000000000000 ) ) 
 REPRESENTATION_ITEM ( '' )  );
#1898 = CARTESIAN_POINT ( 'NONE',  ( 4.999999999999997335, 0.000000000000000000, 4.250000000000000000 ) ) ;
#1899 = ORIENTED_EDGE ( 'NONE', *, *, #3507, .T. ) ;
#1900 = VECTOR ( 'NONE', #1311, 1000.000000000000000 ) ;
#1901 = DIRECTION ( 'NONE',  ( -0.7071067811865537900, -0.4999999999999972800, 0.4999999999999940603 ) ) ;
#1902 = ORIENTED_EDGE ( 'NONE', *, *, #8070, .F. ) ;
#1903 = ADVANCED_FACE ( 'NONE', ( #15663 ), #8032, .T. ) ;
#1904 = PLANE ( 'NONE',  #3742 ) ;
#1905 = DIRECTION ( 'NONE',  ( 1.000000000000000000, 0.000000000000000000, 0.000000000000000000 ) ) ;
#1906 = CARTESIAN_POINT ( 'NONE',  ( -41.00000000000000711, 53.00000000000000711, -44.00000000000000000 ) ) ;
#1907 = DIRECTION ( 'NONE',  ( 0.000000000000000000, 0.000000000000000000, -1.000000000000000000 ) ) ;
#1908 = AXIS2_PLACEMENT_3D ( 'NONE', #13111, #10073, #8704 ) ;
#1909 = DIRECTION ( 'NONE',  ( -0.000000000000000000, -0.000000000000000000, -1.000000000000000000 ) ) ;
#1910 = LINE ( 'NONE', #4658, #1118 ) ;
#1911 = VECTOR ( 'NONE', #16871, 1000.000000000000000 ) ;
#1912 = ORIENTED_EDGE ( 'NONE', *, *, #10203, .T. ) ;
#1913 = DIRECTION ( 'NONE',  ( 1.000000000000000000, 0.000000000000000000, 0.000000000000000000 ) ) ;
#1914 = CIRCLE ( 'NONE', #12851, 1.599999999999997202 ) ;
#1915 = CARTESIAN_POINT ( 'NONE',  ( -11.21908421996108629, -20.46040770435011069, 20.66992750791695244 ) ) ;
#1916 = CARTESIAN_POINT ( 'NONE',  ( 1.035533905932738197, 66.50000000000000000, 45.85000000218494165 ) ) ;
#1917 = CARTESIAN_POINT ( 'NONE',  ( -18.53959229564982536, -27.78091578003890660, 14.76757249208303691 ) ) ;
#1918 = VECTOR ( 'NONE', #946, 1000.000000000000000 ) ;
#1919 = EDGE_CURVE ( 'NONE', #7133, #14697, #1230, .T. ) ;
#1920 = LINE ( 'NONE', #12489, #9763 ) ;
#1921 = EDGE_CURVE ( 'NONE', #2736, #14967, #6558, .T. ) ;
#1922 = CARTESIAN_POINT ( 'NONE',  ( -19.95583473709191580, -22.49542703274176603, 13.66992750791695599 ) ) ;
#1923 = CARTESIAN_POINT ( 'NONE',  ( -1.530808498934192803E-16, 66.50000000000000000, 44.30000000218494449 ) ) ;
#1924 = CARTESIAN_POINT ( 'NONE',  ( -11.21908421996108984, -20.46040770435011069, 20.66992750791695599 ) ) ;
#1925 = FACE_OUTER_BOUND ( 'NONE', #17623, .T. ) ;
#1926 = CARTESIAN_POINT ( 'NONE',  ( -25.00000000000000000, 53.00000000000000711, 30.00000000000000000 ) ) ;
#1927 = AXIS2_PLACEMENT_3D ( 'NONE', #19199, #10259, #10364 ) ;
#1928 = CARTESIAN_POINT ( 'NONE',  ( 0.8561741729129472844, 61.93301270000000613, 48.40000000109247225 ) ) ;
#1929 = DIRECTION ( 'NONE',  ( 0.000000000000000000, 0.000000000000000000, -1.000000000000000000 ) ) ;
#1930 = CARTESIAN_POINT ( 'NONE',  ( -15.00000000000000000, 0.000000000000000000, 7.499999999999995559 ) ) ;
#1931 = AXIS2_PLACEMENT_3D ( 'NONE', #19330, #11859, #9026 ) ;
#1932 = CARTESIAN_POINT ( 'NONE',  ( 3.000000000000000000, 0.000000000000000000, -1.600000000000000311 ) ) ;
#1933 = CARTESIAN_POINT ( 'NONE',  ( -1.461580736456473906, 65.46158073645646880, 48.85000000109246798 ) ) ;
#1934 = CARTESIAN_POINT ( 'NONE',  ( 24.99999999999998579, 0.000000000000000000, 47.49999999999997868 ) ) ;
#1935 = ORIENTED_EDGE ( 'NONE', *, *, #14860, .F. ) ;
#1936 = EDGE_LOOP ( 'NONE', ( #19049, #9020, #5575, #522 ) ) ;
#1937 = CARTESIAN_POINT ( 'NONE',  ( -7.999999999999996447, -23.83517299489733432, 28.54882249208303691 ) ) ;
#1938 = CARTESIAN_POINT ( 'NONE',  ( -12.35725562635140307, -28.24771351637085459, 13.67382249208304223 ) ) ;
#1939 = ORIENTED_EDGE ( 'NONE', *, *, #18111, .F. ) ;
#1940 = CARTESIAN_POINT ( 'NONE',  ( -12.92450931948788906, -26.31681416490114245, 32.48242750791695954 ) ) ;
#1941 = CARTESIAN_POINT ( 'NONE',  ( -41.99999999999997868, 139.6861997365471950, -52.00000000000000000 ) ) ;
#1942 = EDGE_CURVE ( 'NONE', #18922, #13196, #12525, .T. ) ;
#1943 = CARTESIAN_POINT ( 'NONE',  ( -14.83517299489734853, -30.99999999999998224, 19.36132249208304046 ) ) ;
#1944 = VECTOR ( 'NONE', #3202, 1000.000000000000000 ) ;
#1945 = CARTESIAN_POINT ( 'NONE',  ( 0.8561741729129460632, 66.06698729999999387, 47.70000000109248361 ) ) ;
#1946 = CARTESIAN_POINT ( 'NONE',  ( 2.066987300000001415, 64.00000000000000000, 45.95000000109246940 ) ) ;
#1947 = ORIENTED_EDGE ( 'NONE', *, *, #10082, .T. ) ;
#1948 = ORIENTED_EDGE ( 'NONE', *, *, #18362, .F. ) ;
#1949 = CARTESIAN_POINT ( 'NONE',  ( -47.00000000000001421, 30.00000000000000355, 43.75735931288070191 ) ) ;
#1950 = LINE ( 'NONE', #8223, #12571 ) ;
#1951 = PLANE ( 'NONE',  #9058 ) ;
#1952 = ADVANCED_FACE ( 'NONE', ( #14095 ), #6654, .T. ) ;
#1953 = CARTESIAN_POINT ( 'NONE',  ( 1.461580736456473906, 62.53841926354353120, 45.25000000109247367 ) ) ;
#1954 = CARTESIAN_POINT ( 'NONE',  ( 50.00000000000000000, 3.000000000000000000, -60.00000000000000000 ) ) ;
#1955 = DIRECTION ( 'NONE',  ( -1.000000000000000000, -0.000000000000000000, -0.000000000000000000 ) ) ;
#1956 = ORIENTED_EDGE ( 'NONE', *, *, #12876, .F. ) ;
#1958 = EDGE_LOOP ( 'NONE', ( #17310, #17326, #17985, #14474 ) ) ;
#1957 = ORIENTED_EDGE ( 'NONE', *, *, #3607, .F. ) ;
#1959 = CARTESIAN_POINT ( 'NONE',  ( -20.97976432393977575, -20.35725562635143504, 29.63867750791695954 ) ) ;
#1960 = VERTEX_POINT ( 'NONE', #3801 ) ;
#1961 = ORIENTED_EDGE ( 'NONE', *, *, #10797, .F. ) ;
#1962 = CARTESIAN_POINT ( 'NONE',  ( -11.95583473709190514, -24.63902057219072361, 34.01757249208304046 ) ) ;
#1963 = CARTESIAN_POINT ( 'NONE',  ( -8.855408670957631401, -20.64274437364852943, 15.63867750791696132 ) ) ;
#1964 = EDGE_CURVE ( 'NONE', #9967, #3035, #9767, .T. ) ;
#1965 = AXIS2_PLACEMENT_3D ( 'NONE', #17931, #275, #5869 ) ;
#1966 = CARTESIAN_POINT ( 'NONE',  ( 3.796994071234847710E-16, 61.93301269999999903, 48.15000000109247225 ) ) ;
#1967 = CARTESIAN_POINT ( 'NONE',  ( -35.00000000000002132, -0.000000000000000000, -42.50000000000001421 ) ) ;
#1968 = ORIENTED_EDGE ( 'NONE', *, *, #14647, .F. ) ;
#1969 = EDGE_CURVE ( 'NONE', #17858, #7133, #10591, .T. ) ;
#1970 = CARTESIAN_POINT ( 'NONE',  ( -17.95583473709191580, -23.03132541760400898, 13.66992750791696309 ) ) ;
#1971 = DIRECTION ( 'NONE',  ( 0.000000000000000000, 1.000000000000000000, 0.000000000000000000 ) ) ;
#1972 = ORIENTED_EDGE ( 'NONE', *, *, #16364, .F. ) ;
#1973 = FACE_OUTER_BOUND ( 'NONE', #5364, .T. ) ;
#1974 = ORIENTED_EDGE ( 'NONE', *, *, #12424, .T. ) ;
#1975 = DIRECTION ( 'NONE',  ( 0.000000000000000000, 0.000000000000000000, 1.000000000000000000 ) ) ;
#1976 = CARTESIAN_POINT ( 'NONE',  ( -1.035533905932738641, 66.50000000000000000, 46.64999999999999858 ) ) ;
#1977 = CARTESIAN_POINT ( 'NONE',  ( 0.000000000000000000, 0.000000000000000000, 0.000000000000000000 ) ) ;
#1978 = PLANE ( 'NONE',  #14364 ) ;
#1979 = DIRECTION ( 'NONE',  ( 0.000000000000000000, 0.000000000000000000, -1.000000000000000000 ) ) ;
#1980 = CARTESIAN_POINT ( 'NONE',  ( -1.461580736456473906, 65.46158073645646880, 48.65000000109247225 ) ) ;
#1981 = CARTESIAN_POINT ( 'NONE',  ( -6.528048594804062965, -42.28611686177728046, 1.500000000000000000 ) ) ;
#1982 = CARTESIAN_POINT ( 'NONE',  ( -45.00000000000000000, 3.000000000000000000, 56.49999999999998579 ) ) ;
#1983 = DIRECTION ( 'NONE',  ( 1.000000000000000000, -0.000000000000000000, -0.000000000000000000 ) ) ;
#1984 = DIRECTION ( 'NONE',  ( -0.000000000000000000, 0.8660254037844391517, 0.4999999999999991673 ) ) ;
#1985 = EDGE_LOOP ( 'NONE', ( #1083, #16673, #18572, #9771 ) ) ;
#1986 = CARTESIAN_POINT ( 'NONE',  ( -9.955834737091912245, -22.82508104294696594, 26.35742750791695954 ) ) ;
#1987 = DIRECTION ( 'NONE',  ( -1.000000000000000000, 0.000000000000000000, -0.000000000000000000 ) ) ;
#1988 = EDGE_LOOP ( 'NONE', ( #16561, #406, #2501, #11462 ) ) ;
#1989 = CARTESIAN_POINT ( 'NONE',  ( -19.95583473709190514, -25.50457296725822687, 20.45507249208304401 ) ) ;
#1990 = ADVANCED_FACE ( 'NONE', ( #4281 ), #10241, .F. ) ;
#1991 = CARTESIAN_POINT ( 'NONE',  ( -12.92450931948790149, -21.68318583509881137, 22.64257249208304401 ) ) ;
#1992 = FACE_OUTER_BOUND ( 'NONE', #7834, .T. ) ;
#1993 = ORIENTED_EDGE ( 'NONE', *, *, #420, .F. ) ;
#1994 = CARTESIAN_POINT ( 'NONE',  ( 5.199999999999996625, 0.000000000000000000, 0.000000000000000000 ) ) ;
#1995 = ORIENTED_EDGE ( 'NONE', *, *, #6514, .F. ) ;
#1996 = LINE ( 'NONE', #7982, #621 ) ;
#1997 = DIRECTION ( 'NONE',  ( 0.000000000000000000, 0.7071067811865492381, -0.7071067811865457964 ) ) ;
#1998 = LINE ( 'NONE', #13856, #2231 ) ;
#1999 = CARTESIAN_POINT ( 'NONE',  ( -1.265664690411616068E-16, 66.06698730000000808, 44.75000000109247367 ) ) ;
#2000 = CARTESIAN_POINT ( 'NONE',  ( -41.00000000000000711, 53.00000000000000711, -45.00000000000000000 ) ) ;
#2001 = DIRECTION ( 'NONE',  ( -0.000000000000000000, 1.000000000000000000, -0.000000000000000000 ) ) ;
#2002 = PLANE ( 'NONE',  #13642 ) ;
#2003 = EDGE_CURVE ( 'NONE', #6543, #16247, #14565, .T. ) ;
#2004 = VERTEX_POINT ( 'NONE', #9942 ) ;
#2005 = CARTESIAN_POINT ( 'NONE',  ( -9.999999999999994671, -24.16482700510257686, 16.07617750791695954 ) ) ;
#2006 = CARTESIAN_POINT ( 'NONE',  ( 1.767766952966370653, 62.23223304703363112, 44.80000000218493739 ) ) ;
#2007 = CARTESIAN_POINT ( 'NONE',  ( -9.955834737091903364, -25.17491895705294880, 13.01757249208304223 ) ) ;
#2008 =( GEOMETRIC_REPRESENTATION_CONTEXT ( 3 ) GLOBAL_UNCERTAINTY_ASSIGNED_CONTEXT ( ( #3951 ) ) GLOBAL_UNIT_ASSIGNED_CONTEXT ( ( #4036, #14825, #15019 ) ) REPRESENTATION_CONTEXT ( 'NONE', 'WORKASPACE' ) );
#2009 = CARTESIAN_POINT ( 'NONE',  ( -40.00000000000000000, 53.00000000000000711, -19.00000000000000000 ) ) ;
#2010 = ADVANCED_FACE ( 'NONE', ( #14469 ), #14659, .T. ) ;
#2011 = CARTESIAN_POINT ( 'NONE',  ( -12.64274437364855252, -28.41254052147347053, 11.70117750791695777 ) ) ;
#2012 = DIRECTION ( 'NONE',  ( -1.000000000000000000, -2.312964634635742957E-16, 0.000000000000000000 ) ) ;
#2013 = CARTESIAN_POINT ( 'NONE',  ( -19.95583473709191225, -22.49542703274176603, 24.16992750791695599 ) ) ;
#2014 = CARTESIAN_POINT ( 'NONE',  ( 2.499999999999996891, 62.96446609406726225, 47.14999999999999147 ) ) ;
#2015 = CARTESIAN_POINT ( 'NONE',  ( -9.955834737091903364, -25.17491895705295235, 28.76757249208304401 ) ) ;
#2016 = CARTESIAN_POINT ( 'NONE',  ( 2.066987300000002303, 63.14382582708705627, 47.70000000109247651 ) ) ;
#2017 = CARTESIAN_POINT ( 'NONE',  ( -1.035533905932738863, 61.50000000000000000, 49.35000000000000853 ) ) ;
#2018 = LINE ( 'NONE', #18305, #15413 ) ;
#2019 = DIRECTION ( 'NONE',  ( -1.000000000000000000, 0.000000000000000000, -0.000000000000000000 ) ) ;
#2020 = CARTESIAN_POINT ( 'NONE',  ( -2.066987300000001415, 64.00000000000000000, 47.35000000109246798 ) ) ;
#2021 = DIRECTION ( 'NONE',  ( -0.000000000000000000, 1.000000000000000000, -0.000000000000000000 ) ) ;
#2022 = PRESENTATION_LAYER_ASSIGNMENT (  '', '', ( #13275 ) ) ;
#2023 = VECTOR ( 'NONE', #13859, 1000.000000000000000 ) ;
#2024 = EDGE_LOOP ( 'NONE', ( #17054, #11269, #614, #1864 ) ) ;
#2025 = ORIENTED_EDGE ( 'NONE', *, *, #8424, .T. ) ;
#2026 = CARTESIAN_POINT ( 'NONE',  ( -20.24501739517669563, -18.99630608921239627, 26.58007249208304046 ) ) ;
#2027 = CARTESIAN_POINT ( 'NONE',  ( -19.99999999999999645, -24.16482700510261949, 15.42382249208304046 ) ) ;
#2028 = VERTEX_POINT ( 'NONE', #13078 ) ;
#2029 = CARTESIAN_POINT ( 'NONE',  ( -17.07549068051210739, -21.68318583509881847, 29.85742750791696309 ) ) ;
#2030 = CARTESIAN_POINT ( 'NONE',  ( 0.7910017786515960436, 62.09035273295529578, 44.99999999999998579 ) ) ;
#2031 = CARTESIAN_POINT ( 'NONE',  ( -11.64274437364859693, -17.85540867095757989, 17.17382249208304046 ) ) ;
#2032 = CARTESIAN_POINT ( 'NONE',  ( 0.8561741729129472844, 61.93301270000000613, 46.60000000109246088 ) ) ;
#2033 = CARTESIAN_POINT ( 'NONE',  ( -0.8561741729129461742, 66.06698729999999387, 47.00000000109247367 ) ) ;
#2034 = ORIENTED_EDGE ( 'NONE', *, *, #16815, .F. ) ;
#2035 = ORIENTED_EDGE ( 'NONE', *, *, #2635, .T. ) ;
#2036 = AXIS2_PLACEMENT_3D ( 'NONE', #18292, #10618, #3283 ) ;
#2037 = CARTESIAN_POINT ( 'NONE',  ( 2.500000000000001776, 65.03553390593273775, 45.75000000218494733 ) ) ;
#2038 = DIRECTION ( 'NONE',  ( -1.156482317317871478E-16, 1.000000000000000000, 0.000000000000000000 ) ) ;
#2039 = VECTOR ( 'NONE', #16607, 1000.000000000000000 ) ;
#2040 = DIRECTION ( 'NONE',  ( -2.081668171172167774E-16, 0.000000000000000000, 1.000000000000000000 ) ) ;
#2041 = LINE ( 'NONE', #17136, #1550 ) ;
#2042 = DIRECTION ( 'NONE',  ( -1.000000000000000000, 0.000000000000000000, -9.251858538542970348E-17 ) ) ;
#2043 = CARTESIAN_POINT ( 'NONE',  ( -2.315774708385978098, 27.80336399182263563, 58.32836399182264131 ) ) ;
#2044 = CARTESIAN_POINT ( 'NONE',  ( 0.2500000000000002220, 0.000000000000000000, 0.000000000000000000 ) ) ;
#2045 = ORIENTED_EDGE ( 'NONE', *, *, #13819, .T. ) ;
#2046 = ORIENTED_EDGE ( 'NONE', *, *, #9532, .F. ) ;
#2047 = CARTESIAN_POINT ( 'NONE',  ( -9.996306089212364299, -29.24501739517662813, 27.23242750791696309 ) ) ;
#2048 = TOROIDAL_SURFACE ( 'NONE', #502, 2.600000000000000089, 0.1499999999999999944 ) ;
#2049 = CARTESIAN_POINT ( 'NONE',  ( -41.00000000000000711, 110.0000000000000000, 26.50000000000000000 ) ) ;
#2050 = VERTEX_POINT ( 'NONE', #2703 ) ;
#2051 = VECTOR ( 'NONE', #14820, 1000.000000000000000 ) ;
#2052 = VERTEX_POINT ( 'NONE', #10135 ) ;
#2053 = CARTESIAN_POINT ( 'NONE',  ( -17.07549068051208963, -26.31681416490115311, 25.26757249208305112 ) ) ;
#2054 = EDGE_CURVE ( 'NONE', #19239, #2533, #5370, .T. ) ;
#2055 = EDGE_CURVE ( 'NONE', #1767, #12537, #943, .T. ) ;
#2056 = CARTESIAN_POINT ( 'NONE',  ( -9.754982604823348780, -18.99630608921234654, 15.41992750791695777 ) ) ;
#2057 = CARTESIAN_POINT ( 'NONE',  ( 5.799326430397229615, 29.65377616443619857, 56.83055285973290438 ) ) ;
#2058 = CARTESIAN_POINT ( 'NONE',  ( 2.066987300000001859, 63.14382582708704916, 48.30000000109247082 ) ) ;
#2059 = CARTESIAN_POINT ( 'NONE',  ( -24.00000000000000000, 110.0000000000000000, 19.99999999999999645 ) ) ;
#2060 = ORIENTED_EDGE ( 'NONE', *, *, #1237, .F. ) ;
#2061 = CARTESIAN_POINT ( 'NONE',  ( -17.68048971390461688, -25.35725562635141372, 34.01367750791696665 ) ) ;
#2062 = EDGE_CURVE ( 'NONE', #17825, #12973, #3886, .T. ) ;
#2063 =( NAMED_UNIT ( * ) SI_UNIT ( $, .STERADIAN. ) SOLID_ANGLE_UNIT ( ) );
#2064 = ORIENTED_EDGE ( 'NONE', *, *, #8373, .F. ) ;
#2065 = LINE ( 'NONE', #8056, #13773 ) ;
#2066 = ORIENTED_EDGE ( 'NONE', *, *, #14389, .F. ) ;
#2067 = LINE ( 'NONE', #7958, #15703 ) ;
#2068 = APPLICATION_CONTEXT ( 'automotive_design' ) ;
#2069 = PLANE ( 'NONE',  #8114 ) ;
#2070 = DIRECTION ( 'NONE',  ( 0.000000000000000000, 0.000000000000000000, -1.000000000000000000 ) ) ;
#2071 = ADVANCED_FACE ( 'NONE', ( #11707, #17502 ), #7016, .F. ) ;
#2072 = DIRECTION ( 'NONE',  ( 0.000000000000000000, 0.000000000000000000, -1.000000000000000000 ) ) ;
#2073 = VECTOR ( 'NONE', #14569, 1000.000000000000000 ) ;
#2074 = DIRECTION ( 'NONE',  ( 0.000000000000000000, 0.000000000000000000, -1.000000000000000000 ) ) ;
#2075 = VECTOR ( 'NONE', #6244, 1000.000000000000000 ) ;
#2076 = LINE ( 'NONE', #12065, #18989 ) ;
#2077 = DIRECTION ( 'NONE',  ( -0.000000000000000000, -1.000000000000000000, -0.000000000000000000 ) ) ;
#2078 = DIRECTION ( 'NONE',  ( -7.602811950582247805E-15, 0.000000000000000000, 1.000000000000000000 ) ) ;
#2079 = DIRECTION ( 'NONE',  ( -5.782411586589357392E-17, 0.000000000000000000, -1.000000000000000000 ) ) ;
#2080 = VERTEX_POINT ( 'NONE', #12985 ) ;
#2081 = EDGE_CURVE ( 'NONE', #18230, #8527, #14279, .T. ) ;
#2082 = CARTESIAN_POINT ( 'NONE',  ( -10.58745947852649927, -21.64274437364853654, 31.38867750791696309 ) ) ;
#2083 = CARTESIAN_POINT ( 'NONE',  ( 0.000000000000000000, -32.00000000000000711, 1.500000000000000000 ) ) ;
#2084 = EDGE_LOOP ( 'NONE', ( #9328, #14077, #5381, #1326 ) ) ;
#2085 = CARTESIAN_POINT ( 'NONE',  ( -19.41254052147350961, -21.64274437364857562, 36.86132249208304046 ) ) ;
#2086 = VECTOR ( 'NONE', #18460, 1000.000000000000000 ) ;
#2087 = AXIS2_PLACEMENT_3D ( 'NONE', #7003, #18970, #1324 ) ;
#2088 = EDGE_CURVE ( 'NONE', #3058, #16441, #8492, .T. ) ;
#2089 = CARTESIAN_POINT ( 'NONE',  ( -12.31951028609536536, -25.35725562635139596, 39.48632249208304756 ) ) ;
#2090 = DIRECTION ( 'NONE',  ( -0.000000000000000000, -1.000000000000000000, -0.000000000000000000 ) ) ;
#2091 = EDGE_LOOP ( 'NONE', ( #710, #277, #8234, #7127 ) ) ;
#2092 = CARTESIAN_POINT ( 'NONE',  ( -50.00000000000002132, 33.00000000000000000, 44.99999999999999289 ) ) ;
#2093 = ORIENTED_EDGE ( 'NONE', *, *, #11143, .F. ) ;
#2094 = DIRECTION ( 'NONE',  ( 8.659560562354847809E-17, -1.000000000000000000, -1.221245327087672194E-14 ) ) ;
#2095 = CARTESIAN_POINT ( 'NONE',  ( 4.592425496802577917E-16, 61.50000000000000000, 46.19999999999999574 ) ) ;
#2096 = CARTESIAN_POINT ( 'NONE',  ( -9.673552776372430100E-15, 29.74264068711928743, 48.25735931288073033 ) ) ;
#2097 = DIRECTION ( 'NONE',  ( 0.000000000000000000, 0.7071067811865456854, 0.7071067811865494601 ) ) ;
#2098 = AXIS2_PLACEMENT_3D ( 'NONE', #6306, #15604, #1892 ) ;
#2099 = EDGE_CURVE ( 'NONE', #17064, #8108, #14045, .T. ) ;
#2100 = AXIS2_PLACEMENT_3D ( 'NONE', #12458, #507, #9517 ) ;
#2101 = EDGE_CURVE ( 'NONE', #16545, #10270, #8584, .T. ) ;
#2102 = LINE ( 'NONE', #16904, #758 ) ;
#2103 = DIRECTION ( 'NONE',  ( 0.000000000000000000, 0.000000000000000000, 1.000000000000000000 ) ) ;
#2104 = FACE_OUTER_BOUND ( 'NONE', #8312, .T. ) ;
#2105 = ORIENTED_EDGE ( 'NONE', *, *, #7810, .T. ) ;
#2106 = ADVANCED_FACE ( 'NONE', ( #7115 ), #19078, .T. ) ;
#2107 = CARTESIAN_POINT ( 'NONE',  ( -13.82508104294698192, -29.04416526290806644, 27.66992750791695244 ) ) ;
#2108 = CARTESIAN_POINT ( 'NONE',  ( -1.035533905932738641, 66.50000000000000000, 46.75000000218494733 ) ) ;
#2109 = CARTESIAN_POINT ( 'NONE',  ( -10.04416526290808953, -22.49542703274172695, 12.58007249208304046 ) ) ;
#2110 = DIRECTION ( 'NONE',  ( -0.000000000000000000, -1.000000000000000000, -0.000000000000000000 ) ) ;
#2111 = CARTESIAN_POINT ( 'NONE',  ( -10.58745947852649927, -21.64274437364853654, 10.38867750791695777 ) ) ;
#2112 = DIRECTION ( 'NONE',  ( 0.000000000000000000, 0.000000000000000000, -1.000000000000000000 ) ) ;
#2113 = CARTESIAN_POINT ( 'NONE',  ( -12.35725562635143682, -19.75228648362908501, 25.70117750791695599 ) ) ;
#2114 = CARTESIAN_POINT ( 'NONE',  ( -1.767766952966369765, 62.23223304703363112, 46.89999999999999858 ) ) ;
#2115 = CARTESIAN_POINT ( 'NONE',  ( -11.46040770435015332, -20.21908421996104011, 27.89257249208303691 ) ) ;
#2116 = EDGE_CURVE ( 'NONE', #10863, #4229, #17606, .T. ) ;
#2117 = CARTESIAN_POINT ( 'NONE',  ( -2.500000000000001776, 64.00000000000000000, 48.39999999999999858 ) ) ;
#2118 = DIRECTION ( 'NONE',  ( 8.673617379884027583E-16, -1.000000000000000000, 0.000000000000000000 ) ) ;
#2119 = CARTESIAN_POINT ( 'NONE',  ( -3.400000000000017675, 29.47747564417433352, 56.65425233947095052 ) ) ;
#2120 = CARTESIAN_POINT ( 'NONE',  ( -24.00000000000000000, 110.0000000000000000, 30.00000000000000000 ) ) ;
#2121 = CARTESIAN_POINT ( 'NONE',  ( 1.461580736456473906, 62.53841926354353120, 46.85000000109246798 ) ) ;
#2122 = LINE ( 'NONE', #11210, #17713 ) ;
#2123 =( BOUNDED_CURVE ( )  B_SPLINE_CURVE ( 2, ( #18705, #9940, #5551, #15758, #11415, #5647, #17499, #2319, #1038 ),
 .UNSPECIFIED., .F., .F. ) 
 B_SPLINE_CURVE_WITH_KNOTS ( ( 3, 2, 2, 2, 3 ),
 ( 0.6428571428571429047, 0.6607142857142856984, 0.6785714285714286031, 0.6964285714285712858, 0.7142857142857141906 ),
 .UNSPECIFIED. ) 
 CURVE ( )  GEOMETRIC_REPRESENTATION_ITEM ( )  RATIONAL_B_SPLINE_CURVE ( ( 1.000000000000000000, 0.9238795325112867385, 1.000000000000000000, 0.9238795325112867385, 1.000000000000000000, 0.9238795325112867385, 1.000000000000000000, 0.9238795325112871826, 0.9999999999999995559 ) ) 
 REPRESENTATION_ITEM ( '' )  );
#2124 = EDGE_LOOP ( 'NONE', ( #2728, #6832, #19211, #11058 ) ) ;
#2125 = CARTESIAN_POINT ( 'NONE',  ( -9.754982604823302594, -29.00369391078756465, 34.45507249208304046 ) ) ;
#2126 = CARTESIAN_POINT ( 'NONE',  ( -10.04416526290808598, -22.49542703274172695, 12.58007249208304046 ) ) ;
#2127 = CARTESIAN_POINT ( 'NONE',  ( -11.95583473709191047, -23.36097942780921954, 26.35742750791696309 ) ) ;
#2128 = DIRECTION ( 'NONE',  ( 0.000000000000000000, 0.000000000000000000, -1.000000000000000000 ) ) ;
#2129 = CARTESIAN_POINT ( 'NONE',  ( -9.754982604823302594, -29.00369391078756465, 23.95507249208304046 ) ) ;
#2130 = CARTESIAN_POINT ( 'NONE',  ( 1.461580736456473684, 65.46158073645646880, 47.65000000109247225 ) ) ;
#2131 = CARTESIAN_POINT ( 'NONE',  ( -1.040834085586084257E-14, -42.00099999999996214, -15.00100000000031208 ) ) ;
#2132 = ORIENTED_EDGE ( 'NONE', *, *, #64, .T. ) ;
#2133 = ORIENTED_EDGE ( 'NONE', *, *, #10715, .T. ) ;
#2134 = DIRECTION ( 'NONE',  ( 0.000000000000000000, 1.000000000000000000, 0.000000000000000000 ) ) ;
#2135 = CARTESIAN_POINT ( 'NONE',  ( 2.500000000000000000, -1.178949249685218970, -2.041999999999998039 ) ) ;
#2136 = ADVANCED_FACE ( 'NONE', ( #8678 ), #2411, .F. ) ;
#2137 = FACE_OUTER_BOUND ( 'NONE', #3926, .T. ) ;
#2138 = CARTESIAN_POINT ( 'NONE',  ( -2.500000000000001776, 64.00000000000000000, 49.99999999999999289 ) ) ;
#2139 = CARTESIAN_POINT ( 'NONE',  ( -1.461580736456473906, 65.46158073645646880, 44.85000000109246798 ) ) ;
#2140 = FACE_OUTER_BOUND ( 'NONE', #5028, .T. ) ;
#2141 = LINE ( 'NONE', #8128, #7061 ) ;
#2142 = ORIENTED_EDGE ( 'NONE', *, *, #16219, .F. ) ;
#2143 = VERTEX_POINT ( 'NONE', #19176 ) ;
#2144 = CARTESIAN_POINT ( 'NONE',  ( -12.95952864787955150, -17.04416526290805933, 30.73242750791696309 ) ) ;
#2145 = ORIENTED_EDGE ( 'NONE', *, *, #1820, .F. ) ;
#2147 = ORIENTED_EDGE ( 'NONE', *, *, #3502, .F. ) ;
#2146 = VERTEX_POINT ( 'NONE', #17702 ) ;
#2148 = CARTESIAN_POINT ( 'NONE',  ( -12.92450931948790149, -21.68318583509881137, 38.39257249208304756 ) ) ;
#2149 = CARTESIAN_POINT ( 'NONE',  ( -21.99999999999999289, -23.83517299489739116, 18.70117750791695599 ) ) ;
#2150 = VECTOR ( 'NONE', #11508, 1000.000000000000000 ) ;
#2151 = CARTESIAN_POINT ( 'NONE',  ( -1.767766952966370209, 65.76776695296638309, 47.49999999999999289 ) ) ;
#2152 = CARTESIAN_POINT ( 'NONE',  ( -2.500000000000000888, 62.96446609406726935, 47.75000000218494023 ) ) ;
#2153 = CARTESIAN_POINT ( 'NONE',  ( -41.00000000000000711, 110.0000000000000000, -25.50000000000000000 ) ) ;
#2154 = EDGE_LOOP ( 'NONE', ( #4620, #3031, #1261, #11245 ) ) ;
#2155 = CARTESIAN_POINT ( 'NONE',  ( -15.63902057219076269, -20.95583473709189448, 25.04492750791696309 ) ) ;
#2156 = PRESENTATION_STYLE_ASSIGNMENT (( #12547 ) ) ;
#2157 = EDGE_LOOP ( 'NONE', ( #18218, #13220, #5391, #13980, #3183 ) ) ;
#2158 = CARTESIAN_POINT ( 'NONE',  ( -41.00000000000000711, 53.00000000000000711, -6.000000000000001776 ) ) ;
#2159 = VERTEX_POINT ( 'NONE', #12797 ) ;
#2160 = DIRECTION ( 'NONE',  ( 1.000000000000000000, 0.000000000000000000, 0.000000000000000000 ) ) ;
#2161 = CARTESIAN_POINT ( 'NONE',  ( -2.500000000000001776, 64.00000000000000000, 45.19999999999999574 ) ) ;
#2162 = CARTESIAN_POINT ( 'NONE',  ( -40.00000000000000000, 52.00000000000000711, 30.00000000000000000 ) ) ;
#2163 = CIRCLE ( 'NONE', #9081, 2.600000000000000089 ) ;
#2164 = DIRECTION ( 'NONE',  ( 0.000000000000000000, -0.5000000000000009992, -0.8660254037844380415 ) ) ;
#2165 = CARTESIAN_POINT ( 'NONE',  ( 1.461580736456473684, 65.46158073645646880, 47.05000000109247082 ) ) ;
#2166 = LINE ( 'NONE', #11258, #13473 ) ;
#2167 = AXIS2_PLACEMENT_3D ( 'NONE', #11686, #8658, #8949 ) ;
#2168 = DIRECTION ( 'NONE',  ( 0.000000000000000000, 0.000000000000000000, 1.000000000000000000 ) ) ;
#2169 = CARTESIAN_POINT ( 'NONE',  ( -10.00000000000000000, -37.50000000000000000, -3.000000000000000000 ) ) ;
#2170 = VERTEX_POINT ( 'NONE', #13675 ) ;
#2171 = CARTESIAN_POINT ( 'NONE',  ( -18.78091578003889950, -27.53959229564985378, 33.79492750791696665 ) ) ;
#2172 = FACE_OUTER_BOUND ( 'NONE', #664, .T. ) ;
#2173 = EDGE_LOOP ( 'NONE', ( #14107, #11827, #15804, #3822 ) ) ;
#2174 = CARTESIAN_POINT ( 'NONE',  ( -10.75228648362912232, -21.35725562635138530, 38.61132249208304046 ) ) ;
#2175 = ADVANCED_FACE ( 'NONE', ( #16633 ), #15159, .F. ) ;
#2176 = VECTOR ( 'NONE', #9853, 1000.000000000000000 ) ;
#2177 = CARTESIAN_POINT ( 'NONE',  ( -14.03132541760400009, -26.95583473709189448, 29.64257249208304401 ) ) ;
#2178 = VECTOR ( 'NONE', #16703, 1000.000000000000000 ) ;
#2179 = ORIENTED_EDGE ( 'NONE', *, *, #16558, .T. ) ;
#2180 = AXIS2_PLACEMENT_3D ( 'NONE', #8702, #9970, #15972 ) ;
#2181 = CARTESIAN_POINT ( 'NONE',  ( -41.00000000000000711, 53.00000000000000711, 21.00000000000000000 ) ) ;
#2182 = ORIENTED_EDGE ( 'NONE', *, *, #18397, .F. ) ;
#2183 = CARTESIAN_POINT ( 'NONE',  ( -2.500000000000001776, 64.00000000000000000, 45.30000000218493739 ) ) ;
#2184 = FACE_OUTER_BOUND ( 'NONE', #3832, .T. ) ;
#2185 = DIRECTION ( 'NONE',  ( 1.000000000000000000, -0.000000000000000000, -0.000000000000000000 ) ) ;
#2186 = EDGE_CURVE ( 'NONE', #3115, #13282, #19372, .T. ) ;
#2187 = AXIS2_PLACEMENT_3D ( 'NONE', #4846, #17003, #15134 ) ;
#2188 = CARTESIAN_POINT ( 'NONE',  ( 4.012830983233651061, 32.52836399182262994, 53.60336399182268252 ) ) ;
#2189 = SURFACE_STYLE_FILL_AREA ( #8271 ) ;
#2190 = DIRECTION ( 'NONE',  ( -1.000000000000000000, -0.000000000000000000, -0.000000000000000000 ) ) ;
#2191 = CARTESIAN_POINT ( 'NONE',  ( -13.49999999999974065, 39.11180553784110003, 47.01992244580424085 ) ) ;
#2192 = UNCERTAINTY_MEASURE_WITH_UNIT (LENGTH_MEASURE( 1.000000000000000082E-05 ), #3374, 'distance_accuracy_value', 'NONE');
#2193 = ORIENTED_EDGE ( 'NONE', *, *, #10563, .F. ) ;
#2194 = CARTESIAN_POINT ( 'NONE',  ( -16.50457296725820555, -28.95583473709189448, 33.35742750791695954 ) ) ;
#2195 = CIRCLE ( 'NONE', #4064, 6.799999999999999822 ) ;
#2196 = CARTESIAN_POINT ( 'NONE',  ( 1.767766952966369987, 65.76776695296638309, 45.80000000218493739 ) ) ;
#2197 = CARTESIAN_POINT ( 'NONE',  ( -18.78091578003892081, -20.46040770435013556, 37.08007249208304046 ) ) ;
#2198 = EDGE_CURVE ( 'NONE', #869, #11368, #7409, .T. ) ;
#2199 = EDGE_CURVE ( 'NONE', #3007, #4393, #13379, .T. ) ;
#2200 = VECTOR ( 'NONE', #3797, 1000.000000000000000 ) ;
#2201 = FACE_OUTER_BOUND ( 'NONE', #18242, .T. ) ;
#2202 = CARTESIAN_POINT ( 'NONE',  ( -9.999999999999994671, -24.16482700510257686, 37.07617750791695954 ) ) ;
#2203 = EDGE_CURVE ( 'NONE', #1661, #2980, #5847, .T. ) ;
#2204 = LINE ( 'NONE', #11019, #3903 ) ;
#2205 = CARTESIAN_POINT ( 'NONE',  ( -12.64274437364855252, -28.41254052147347053, 37.95117750791695954 ) ) ;
#2206 = AXIS2_PLACEMENT_3D ( 'NONE', #3640, #15597, #5215 ) ;
#2207 = DIRECTION ( 'NONE',  ( 1.000000000000000000, 0.000000000000000000, 0.000000000000000000 ) ) ;
#2208 = CARTESIAN_POINT ( 'NONE',  ( -16.17491895705296656, -29.04416526290807354, 19.58007249208303691 ) ) ;
#2209 = CARTESIAN_POINT ( 'NONE',  ( -0.8561741729129461742, 66.06698729999999387, 45.60000000109246088 ) ) ;
#2210 = DIRECTION ( 'NONE',  ( 0.000000000000000000, -1.000000000000000000, 0.000000000000000000 ) ) ;
#2211 = CARTESIAN_POINT ( 'NONE',  ( -7.999999999999986677, 60.00000000000000711, 45.00000000000000000 ) ) ;
#2212 = PRESENTATION_LAYER_ASSIGNMENT (  '', '', ( #4734 ) ) ;
#2213 = CARTESIAN_POINT ( 'NONE',  ( 4.999999999999997335, 5.204748896376250699E-16, -4.250000000000000000 ) ) ;
#2214 = CARTESIAN_POINT ( 'NONE',  ( 1.767766952966370653, 62.23223304703363112, 48.69999999999999574 ) ) ;
#2215 = LINE ( 'NONE', #3970, #7707 ) ;
#2216 = VECTOR ( 'NONE', #9024, 1000.000000000000000 ) ;
#2217 = VERTEX_POINT ( 'NONE', #6047 ) ;
#2218 = PRESENTATION_LAYER_ASSIGNMENT (  '', '', ( #3160 ) ) ;
#2219 = CARTESIAN_POINT ( 'NONE',  ( -2.066987300000001415, 64.00000000000000000, 46.35000000109246798 ) ) ;
#2220 = EDGE_CURVE ( 'NONE', #10469, #11653, #13483, .T. ) ;
#2221 = CARTESIAN_POINT ( 'NONE',  ( -17.68048971390461688, -25.35725562635141372, 23.51367750791696309 ) ) ;
#2222 = EDGE_CURVE ( 'NONE', #1572, #16704, #12004, .T. ) ;
#2223 = LINE ( 'NONE', #1941, #12063 ) ;
#2224 = CARTESIAN_POINT ( 'NONE',  ( -11.35725562635139418, -29.97976432393972601, 29.42382249208304046 ) ) ;
#2225 = VECTOR ( 'NONE', #9876, 1000.000000000000114 ) ;
#2226 = CARTESIAN_POINT ( 'NONE',  ( -2.066987300000001859, 64.85617417291294373, 47.90000000109247225 ) ) ;
#2227 = VERTEX_POINT ( 'NONE', #9174 ) ;
#2228 = ORIENTED_EDGE ( 'NONE', *, *, #12857, .F. ) ;
#2229 = DIRECTION ( 'NONE',  ( 0.000000000000000000, 0.6139406135149196864, -0.7893522173763268812 ) ) ;
#2230 = DIRECTION ( 'NONE',  ( -0.000000000000000000, -1.000000000000000000, -0.000000000000000000 ) ) ;
#2231 = VECTOR ( 'NONE', #5321, 1000.000000000000000 ) ;
#2232 = CARTESIAN_POINT ( 'NONE',  ( -1.265664690411616068E-16, 66.06698730000000808, 45.35000000109246798 ) ) ;
#2233 = DIRECTION ( 'NONE',  ( 0.000000000000000000, 1.000000000000000000, 0.000000000000000000 ) ) ;
#2234 = MECHANICAL_DESIGN_GEOMETRIC_PRESENTATION_REPRESENTATION (  '', ( #1625 ), #17896 ) ;
#2235 = CARTESIAN_POINT ( 'NONE',  ( 1.035533905932739751, 61.50000000000000000, 47.85000000000000142 ) ) ;
#2236 = DIRECTION ( 'NONE',  ( -2.220446049250312588E-16, 0.7071067811865453523, 0.7071067811865496822 ) ) ;
#2237 = VECTOR ( 'NONE', #15155, 1000.000000000000000 ) ;
#2238 = DIRECTION ( 'NONE',  ( 0.000000000000000000, 0.000000000000000000, -1.000000000000000000 ) ) ;
#2239 = VERTEX_POINT ( 'NONE', #10630 ) ;
#2240 = ORIENTED_EDGE ( 'NONE', *, *, #2551, .T. ) ;
#2241 = CARTESIAN_POINT ( 'NONE',  ( -21.99999999999999289, -23.83517299489739116, 29.20117750791695244 ) ) ;
#2242 = VECTOR ( 'NONE', #5458, 1000.000000000000227 ) ;
#2243 = ORIENTED_EDGE ( 'NONE', *, *, #4334, .T. ) ;
#2245 = ORIENTED_EDGE ( 'NONE', *, *, #8811, .F. ) ;
#2244 = ORIENTED_EDGE ( 'NONE', *, *, #1518, .T. ) ;
#2246 = EDGE_CURVE ( 'NONE', #16262, #10297, #6239, .T. ) ;
#2247 = CARTESIAN_POINT ( 'NONE',  ( -11.95583473709190514, -24.63902057219072361, 28.76757249208304401 ) ) ;
#2248 = CARTESIAN_POINT ( 'NONE',  ( -17.04047135212043784, -30.95583473709190159, 17.60742750791695954 ) ) ;
#2249 = VECTOR ( 'NONE', #7326, 1000.000000000000000 ) ;
#2250 = PLANE ( 'NONE',  #19151 ) ;
#2251 = CARTESIAN_POINT ( 'NONE',  ( -2.500000000000001776, 65.03553390593273775, 49.25000000218494023 ) ) ;
#2252 = DIRECTION ( 'NONE',  ( 0.000000000000000000, 0.000000000000000000, -1.000000000000000000 ) ) ;
#2253 = EDGE_LOOP ( 'NONE', ( #7371, #17666, #6169, #5889 ) ) ;
#2254 = CARTESIAN_POINT ( 'NONE',  ( -17.95583473709191580, -23.03132541760400898, 29.41992750791696665 ) ) ;
#2255 = CARTESIAN_POINT ( 'NONE',  ( 41.99999999999997868, 3.000000000000000000, 2.802245615039457371E-15 ) ) ;
#2256 = ORIENTED_EDGE ( 'NONE', *, *, #1237, .T. ) ;
#2257 = DIRECTION ( 'NONE',  ( 0.000000000000000000, 0.000000000000000000, -1.000000000000000000 ) ) ;
#2258 = ORIENTED_EDGE ( 'NONE', *, *, #13660, .T. ) ;
#2259 = DIRECTION ( 'NONE',  ( 0.000000000000000000, -1.000000000000000000, 0.000000000000000000 ) ) ;
#2260 = ADVANCED_FACE ( 'NONE', ( #12105 ), #9336, .F. ) ;
#2261 = CARTESIAN_POINT ( 'NONE',  ( -4.189131392896543460, 32.57932772728320003, 53.90500129688591358 ) ) ;
#2262 = LINE ( 'NONE', #8060, #15938 ) ;
#2263 = CARTESIAN_POINT ( 'NONE',  ( 2.066987300000001415, 64.00000000000000000, 49.15000000109247225 ) ) ;
#2264 = CARTESIAN_POINT ( 'NONE',  ( 0.8561741729129471734, 61.93301270000000613, 46.80000000109247082 ) ) ;
#2265 = CARTESIAN_POINT ( 'NONE',  ( 32.50000000000000000, 52.00000000000000711, 12.50000000000000000 ) ) ;
#2266 = VECTOR ( 'NONE', #15054, 1000.000000000000000 ) ;
#2267 = PLANE ( 'NONE',  #2100 ) ;
#2268 = CARTESIAN_POINT ( 'NONE',  ( -8.528048594804062077, -42.28611686177728046, 1.500000000000000000 ) ) ;
#2269 = VERTEX_POINT ( 'NONE', #2993 ) ;
#2270 = ORIENTED_EDGE ( 'NONE', *, *, #13660, .F. ) ;
#2271 = CARTESIAN_POINT ( 'NONE',  ( -16.17491895705301275, -18.95583473709189803, 35.54492750791695954 ) ) ;
#2272 = FACE_OUTER_BOUND ( 'NONE', #762, .T. ) ;
#2273 = ORIENTED_EDGE ( 'NONE', *, *, #12227, .T. ) ;
#2274 = EDGE_CURVE ( 'NONE', #9587, #17823, #1639, .T. ) ;
#2275 = CARTESIAN_POINT ( 'NONE',  ( -19.99999999999999645, -24.16482700510261949, 25.92382249208304401 ) ) ;
#2276 = CARTESIAN_POINT ( 'NONE',  ( -2.500000000000001776, 64.00000000000000000, 45.19999999999999574 ) ) ;
#2277 = CARTESIAN_POINT ( 'NONE',  ( -15.63902057219073605, -27.04416526290807710, 30.08007249208304401 ) ) ;
#2278 = PLANE ( 'NONE',  #3150 ) ;
#2279 = ORIENTED_EDGE ( 'NONE', *, *, #9499, .F. ) ;
#2280 = DIRECTION ( 'NONE',  ( -0.000000000000000000, -0.000000000000000000, -1.000000000000000000 ) ) ;
#2281 = VERTEX_POINT ( 'NONE', #13274 ) ;
#2282 = DIRECTION ( 'NONE',  ( 0.000000000000000000, 0.000000000000000000, 1.000000000000000000 ) ) ;
#2283 = CARTESIAN_POINT ( 'NONE',  ( -40.00000000000000711, 113.0000000000000000, 1.500000000000001332 ) ) ;
#2284 = CARTESIAN_POINT ( 'NONE',  ( 1.035533905932738197, 66.50000000000000000, 45.85000000218494165 ) ) ;
#2285 = FILL_AREA_STYLE ('',( #11474 ) ) ;
#2286 =( NAMED_UNIT ( * ) PLANE_ANGLE_UNIT ( ) SI_UNIT ( $, .RADIAN. ) );
#2287 = CARTESIAN_POINT ( 'NONE',  ( 11.00000000000002309, 68.00000000000000000, 63.99999999999994316 ) ) ;
#2288 = CARTESIAN_POINT ( 'NONE',  ( 2.492551403682577771, 31.20336399182262710, 54.92836399182266405 ) ) ;
#2289 = VERTEX_POINT ( 'NONE', #10435 ) ;
#2290 = CARTESIAN_POINT ( 'NONE',  ( -9.955834737091912245, -22.82508104294696594, 31.60742750791695954 ) ) ;
#2291 = CARTESIAN_POINT ( 'NONE',  ( 3.796994071234847710E-16, 61.93301269999999903, 47.35000000109246798 ) ) ;
#2292 = EDGE_CURVE ( 'NONE', #5477, #587, #18207, .T. ) ;
#2293 = EDGE_CURVE ( 'NONE', #6744, #15813, #4783, .T. ) ;
#2294 = CARTESIAN_POINT ( 'NONE',  ( -16.17491895705296656, -29.04416526290807710, 35.33007249208301914 ) ) ;
#2295 = CARTESIAN_POINT ( 'NONE',  ( -0.1250000000000104083, 27.33847763108499507, 59.14680374315354783 ) ) ;
#2296 = CARTESIAN_POINT ( 'NONE',  ( -12.35725562635143682, -19.75228648362908501, 30.95117750791695954 ) ) ;
#2297 = EDGE_CURVE ( 'NONE', #8527, #17051, #14859, .T. ) ;
#2298 = CARTESIAN_POINT ( 'NONE',  ( -25.00000000000001421, -6.000000000000000000, 47.49999999999997868 ) ) ;
#2299 = CARTESIAN_POINT ( 'NONE',  ( -20.04416526290808065, -25.17491895705300209, 28.98242750791695599 ) ) ;
#2300 = CARTESIAN_POINT ( 'NONE',  ( 2.500000000000001776, 64.00000000000000000, 46.50000000218494733 ) ) ;
#2301 = CARTESIAN_POINT ( 'NONE',  ( -17.35725562635140307, -28.41254052147349185, 30.29882249208304401 ) ) ;
#2302 = CARTESIAN_POINT ( 'NONE',  ( -2.500000000000000888, 62.96446609406726935, 48.44999999999999574 ) ) ;
#2303 = CARTESIAN_POINT ( 'NONE',  ( -1.265664690411616068E-16, 66.06698730000000808, 49.55000000109247082 ) ) ;
#2304 = CARTESIAN_POINT ( 'NONE',  ( 5.800448907431066559, 29.80092238452519382, 56.68308948419219462 ) ) ;
#2305 = CARTESIAN_POINT ( 'NONE',  ( 1.035533905932739751, 61.50000000000000000, 49.44999999999999574 ) ) ;
#2306 = CARTESIAN_POINT ( 'NONE',  ( -41.00000000000000711, 110.0000000000000000, -12.50000000000000000 ) ) ;
#2307 = EDGE_CURVE ( 'NONE', #14415, #6823, #17804, .T. ) ;
#2308 = VERTEX_POINT ( 'NONE', #4381 ) ;
#2309 = ADVANCED_FACE ( 'NONE', ( #8875 ), #66, .T. ) ;
#2310 = ADVANCED_FACE ( 'NONE', ( #15062 ), #7612, .T. ) ;
#2311 = CARTESIAN_POINT ( 'NONE',  ( -2.066987300000000971, 63.14382582708704916, 45.60000000109246798 ) ) ;
#2312 = CARTESIAN_POINT ( 'NONE',  ( -14.83517299489738761, -20.99999999999997513, 35.76367750791695954 ) ) ;
#2313 = APPLICATION_CONTEXT ( 'automotive_design' ) ;
#2314 = CARTESIAN_POINT ( 'NONE',  ( 4.012830983233651061, 32.52836399182262994, 53.60336399182268252 ) ) ;
#2315 = CARTESIAN_POINT ( 'NONE',  ( -9.754982604823302594, -29.00369391078756465, 39.70507249208304046 ) ) ;
#2316 = CARTESIAN_POINT ( 'NONE',  ( -1.265664690411616068E-16, 66.06698730000000808, 46.15000000109247225 ) ) ;
#2317 = ORIENTED_EDGE ( 'NONE', *, *, #4372, .F. ) ;
#2318 = LINE ( 'NONE', #11505, #5595 ) ;
#2319 = CARTESIAN_POINT ( 'NONE',  ( -2.499999999999996003, 62.96446609406726225, 45.35000000218493454 ) ) ;
#2320 = LINE ( 'NONE', #8304, #8422 ) ;
#2321 = CARTESIAN_POINT ( 'NONE',  ( -6.528048594804062965, -42.28611686177728046, 3.000000000000000000 ) ) ;
#2322 = DIRECTION ( 'NONE',  ( -1.000000000000000000, 0.000000000000000000, -0.000000000000000000 ) ) ;
#2323 = VECTOR ( 'NONE', #7393, 1000.000000000000000 ) ;
#2324 = CARTESIAN_POINT ( 'NONE',  ( -25.00000000000000711, 53.00000000000000711, 0.5000000000000004441 ) ) ;
#2325 = CARTESIAN_POINT ( 'NONE',  ( 1.300000000000000044, 1.478016689125442484, -1.626303258728256651E-15 ) ) ;
#2326 = ADVANCED_FACE ( 'NONE', ( #4674 ), #12498, .F. ) ;
#2327 = EDGE_CURVE ( 'NONE', #16010, #5207, #1831, .T. ) ;
#2328 = CARTESIAN_POINT ( 'NONE',  ( -1.035533905932738863, 61.50000000000000000, 47.74999999999999289 ) ) ;
#2329 = ORIENTED_EDGE ( 'NONE', *, *, #4305, .F. ) ;
#2330 = ORIENTED_EDGE ( 'NONE', *, *, #15528, .F. ) ;
#2331 = CARTESIAN_POINT ( 'NONE',  ( -15.16482700510264436, -16.99999999999997868, 0.9863224920830391262 ) ) ;
#2332 = ORIENTED_EDGE ( 'NONE', *, *, #3099, .F. ) ;
#2334 = ORIENTED_EDGE ( 'NONE', *, *, #9822, .F. ) ;
#2333 = ORIENTED_EDGE ( 'NONE', *, *, #18, .T. ) ;
#2335 = CARTESIAN_POINT ( 'NONE',  ( -15.63902057219073605, -27.04416526290807710, 35.33007249208304046 ) ) ;
#2336 = EDGE_CURVE ( 'NONE', #15781, #15589, #16730, .T. ) ;
#2337 = CARTESIAN_POINT ( 'NONE',  ( -14.83517299489740715, -16.99999999999997868, 25.26367750791695954 ) ) ;
#2338 = MECHANICAL_DESIGN_GEOMETRIC_PRESENTATION_REPRESENTATION (  '', ( #1712 ), #10473 ) ;
#2339 = AXIS2_PLACEMENT_3D ( 'NONE', #16822, #8282, #446 ) ;
#2340 = CARTESIAN_POINT ( 'NONE',  ( -25.00000000000000000, 53.00000000000000711, -18.00000000000000355 ) ) ;
#2341 = CARTESIAN_POINT ( 'NONE',  ( -2.500000000000001776, 64.00000000000000000, 46.10000000218494165 ) ) ;
#2342 = PLANE ( 'NONE',  #1573 ) ;
#2343 = VERTEX_POINT ( 'NONE', #8203 ) ;
#2344 = LINE ( 'NONE', #2618, #661 ) ;
#2345 = VERTEX_POINT ( 'NONE', #9359 ) ;
#2346 = DIRECTION ( 'NONE',  ( 0.000000000000000000, 0.000000000000000000, -1.000000000000000000 ) ) ;
#2347 = ORIENTED_EDGE ( 'NONE', *, *, #1457, .T. ) ;
#2348 = CARTESIAN_POINT ( 'NONE',  ( -1.909647267044692676, 63.20899822134837365, 45.00000000000000000 ) ) ;
#2349 = CARTESIAN_POINT ( 'NONE',  ( -41.00000000000000711, 110.0000000000000000, -5.000000000000000888 ) ) ;
#2350 = DIRECTION ( 'NONE',  ( 0.000000000000000000, -1.000000000000000000, 0.000000000000000000 ) ) ;
#2351 = CARTESIAN_POINT ( 'NONE',  ( -1.265664690411616068E-16, 66.06698730000000808, 49.55000000109247082 ) ) ;
#2352 = EDGE_CURVE ( 'NONE', #18051, #793, #7911, .T. ) ;
#2353 = CARTESIAN_POINT ( 'NONE',  ( -2.066987300000001415, 64.00000000000000000, 47.35000000109246798 ) ) ;
#2354 = LINE ( 'NONE', #10162, #338 ) ;
#2355 = PRODUCT_DEFINITION_FORMATION_WITH_SPECIFIED_SOURCE ( 'ANY', '', #17717, .NOT_KNOWN. ) ;
#2356 = DIRECTION ( 'NONE',  ( 0.000000000000000000, 0.000000000000000000, -1.000000000000000000 ) ) ;
#2357 = CARTESIAN_POINT ( 'NONE',  ( -24.00000000000000711, 53.00000000000000711, -30.99999999999999645 ) ) ;
#2358 = VERTEX_POINT ( 'NONE', #11024 ) ;
#2359 = VERTEX_POINT ( 'NONE', #18499 ) ;
#2360 = CARTESIAN_POINT ( 'NONE',  ( -19.41254052147348830, -26.35725562635142083, 28.76367750791695954 ) ) ;
#2361 = CARTESIAN_POINT ( 'NONE',  ( 0.000000000000000000, 52.00000000000000711, 30.00000000000000000 ) ) ;
#2362 = VERTEX_POINT ( 'NONE', #14169 ) ;
#2363 = CARTESIAN_POINT ( 'NONE',  ( -15.16482700510263371, -18.99999999999997868, 27.23632249208304046 ) ) ;
#2364 = CARTESIAN_POINT ( 'NONE',  ( 1.767766952966370653, 62.23223304703363112, 45.50000000000000000 ) ) ;
#2365 = PRODUCT_RELATED_PRODUCT_CATEGORY ( 'part', '', ( #17717 ) ) ;
#2366 = CARTESIAN_POINT ( 'NONE',  ( -17.31681416490117087, -21.92450931948788551, 31.83007249208304046 ) ) ;
#2367 = VECTOR ( 'NONE', #1595, 1000.000000000000000 ) ;
#2368 = FILL_AREA_STYLE_COLOUR ( '', #5648 ) ;
#2369 = ORIENTED_EDGE ( 'NONE', *, *, #7308, .F. ) ;
#2370 = AXIS2_PLACEMENT_3D ( 'NONE', #8705, #13017, #9888 ) ;
#2371 = DIRECTION ( 'NONE',  ( 0.5773502691896202910, -0.8164965809277299202, 0.000000000000000000 ) ) ;
#2372 = ORIENTED_EDGE ( 'NONE', *, *, #6725, .F. ) ;
#2373 = CARTESIAN_POINT ( 'NONE',  ( -2.492551403682614186, 27.92836399182264273, 58.20336399182264131 ) ) ;
#2374 = DIRECTION ( 'NONE',  ( 1.000000000000000000, -0.000000000000000000, 0.000000000000000000 ) ) ;
#2375 = CARTESIAN_POINT ( 'NONE',  ( 1.000000000000001332, -36.00000000000000711, 4.500000000000000888 ) ) ;
#2376 = CARTESIAN_POINT ( 'NONE',  ( 46.99999999999998579, 6.000000000000000000, 56.99999999999997158 ) ) ;
#2377 = CARTESIAN_POINT ( 'NONE',  ( -15.00000000000000000, -0.000000000000000000, 30.00000000000000000 ) ) ;
#2378 = AXIS2_PLACEMENT_3D ( 'NONE', #6617, #3761, #18579 ) ;
#2379 = PLANE ( 'NONE',  #11132 ) ;
#2380 = ORIENTED_EDGE ( 'NONE', *, *, #2198, .F. ) ;
#2381 = VECTOR ( 'NONE', #19358, 1000.000000000000000 ) ;
#2382 = EDGE_LOOP ( 'NONE', ( #2833, #842, #12674, #5103 ) ) ;
#2383 = CARTESIAN_POINT ( 'NONE',  ( -11.21908421996108629, -20.46040770435011069, 36.41992750791695954 ) ) ;
#2384 = CARTESIAN_POINT ( 'NONE',  ( -2.066987300000001859, 64.85617417291294373, 49.50000000109246656 ) ) ;
#2385 = CARTESIAN_POINT ( 'NONE',  ( -19.95583473709190514, -25.50457296725822687, 30.95507249208303691 ) ) ;
#2386 = CARTESIAN_POINT ( 'NONE',  ( -3.400000000000017675, 29.65425233947097183, 56.47747564417432642 ) ) ;
#2387 = CARTESIAN_POINT ( 'NONE',  ( -18.53959229564986799, -20.21908421996107563, 24.60742750791695954 ) ) ;
#2388 = CARTESIAN_POINT ( 'NONE',  ( 2.500000000000000000, 1.768423874527822459, -1.021000000000002794 ) ) ;
#2389 = AXIS2_PLACEMENT_3D ( 'NONE', #1499, #23, #1599 ) ;
#2390 = CARTESIAN_POINT ( 'NONE',  ( -15.16482700510259640, -28.99999999999998224, 27.88867750791695954 ) ) ;
#2391 = CARTESIAN_POINT ( 'NONE',  ( -50.00000000000002132, 118.0000000000000142, 40.49999999999997868 ) ) ;
#2392 = CARTESIAN_POINT ( 'NONE',  ( -19.41254052147350961, -21.64274437364857562, 31.61132249208303691 ) ) ;
#2393 = CARTESIAN_POINT ( 'NONE',  ( -2.500000000000001776, 65.03553390593273775, 49.14999999999999858 ) ) ;
#2394 = LINE ( 'NONE', #14545, #3079 ) ;
#2395 = LINE ( 'NONE', #8380, #8279 ) ;
#2396 = CARTESIAN_POINT ( 'NONE',  ( 1.035533905932738197, 66.50000000000000000, 49.75000000000000000 ) ) ;
#2397 = ADVANCED_FACE ( 'NONE', ( #5068 ), #3299, .F. ) ;
#2398 = EDGE_CURVE ( 'NONE', #18807, #19283, #18591, .T. ) ;
#2399 = LINE ( 'NONE', #17121, #17102 ) ;
#2400 = ORIENTED_EDGE ( 'NONE', *, *, #2495, .T. ) ;
#2401 = ADVANCED_FACE ( 'NONE', ( #3680 ), #15255, .T. ) ;
#2402 = CARTESIAN_POINT ( 'NONE',  ( 0.8561741729129471734, 61.93301270000000613, 46.60000000109246798 ) ) ;
#2403 = CARTESIAN_POINT ( 'NONE',  ( -17.51566270880201159, -22.35725562635141728, 40.13867750791696665 ) ) ;
#2404 = EDGE_CURVE ( 'NONE', #4659, #7333, #6343, .T. ) ;
#2405 = CARTESIAN_POINT ( 'NONE',  ( -17.04047135212050890, -17.04416526290807710, 32.26757249208304046 ) ) ;
#2406 = CARTESIAN_POINT ( 'NONE',  ( 0.8561741729129460632, 66.06698729999999387, 47.90000000109247225 ) ) ;
#2407 = EDGE_LOOP ( 'NONE', ( #11715, #12132, #2937, #4843 ) ) ;
#2408 = CARTESIAN_POINT ( 'NONE',  ( 2.500000000000000000, 2.357898499370431722, -2.818925648462311528E-15 ) ) ;
#2409 = DIRECTION ( 'NONE',  ( -0.000000000000000000, -1.000000000000000000, -0.000000000000000000 ) ) ;
#2410 = CARTESIAN_POINT ( 'NONE',  ( -2.066987300000001415, 64.85617417291294373, 47.10000000109246798 ) ) ;
#2411 = PLANE ( 'NONE',  #15954 ) ;
#2412 = CARTESIAN_POINT ( 'NONE',  ( -1.767766952966369765, 62.23223304703363112, 47.69999999999999574 ) ) ;
#2413 = DIRECTION ( 'NONE',  ( 3.826732013112563602E-16, -1.000000000000000000, 0.000000000000000000 ) ) ;
#2414 = EDGE_CURVE ( 'NONE', #15895, #11533, #15638, .T. ) ;
#2415 = CARTESIAN_POINT ( 'NONE',  ( -35.00000000000002132, -6.000000000000000000, -47.50000000000002132 ) ) ;
#2416 = VERTEX_POINT ( 'NONE', #7805 ) ;
#2417 = ORIENTED_EDGE ( 'NONE', *, *, #8519, .T. ) ;
#2418 =( REPRESENTATION_RELATIONSHIP ('NONE','NONE', #7912, #15288 ) REPRESENTATION_RELATIONSHIP_WITH_TRANSFORMATION ( #8064 )SHAPE_REPRESENTATION_RELATIONSHIP( ) );
#2419 = CARTESIAN_POINT ( 'NONE',  ( -21.99999999999999289, -23.83517299489739116, 39.70117750791695954 ) ) ;
#2420 = PRESENTATION_STYLE_ASSIGNMENT (( #5189 ) ) ;
#2421 = EDGE_LOOP ( 'NONE', ( #16978, #6316, #18315, #9665 ) ) ;
#2423 = ORIENTED_EDGE ( 'NONE', *, *, #14694, .F. ) ;
#2422 = ORIENTED_EDGE ( 'NONE', *, *, #6658, .F. ) ;
#2424 = CARTESIAN_POINT ( 'NONE',  ( -14.83517299489738761, -20.99999999999997513, -0.9863224920830401254 ) ) ;
#2425 = CARTESIAN_POINT ( 'NONE',  ( -15.16482700510258574, -30.99999999999998224, 27.88867750791695954 ) ) ;
#2426 = CARTESIAN_POINT ( 'NONE',  ( 4.000000000000003553, 47.00000000000000711, 34.99999999999999289 ) ) ;
#2427 = CARTESIAN_POINT ( 'NONE',  ( 2.500000000000002220, 62.96446609406726935, 48.05000000218494449 ) ) ;
#2428 = CARTESIAN_POINT ( 'NONE',  ( -41.00000000000000711, 53.00000000000000711, -38.50000000000000711 ) ) ;
#2429 = ORIENTED_EDGE ( 'NONE', *, *, #6641, .T. ) ;
#2430 = DIRECTION ( 'NONE',  ( -1.000000000000000000, 0.000000000000000000, -0.000000000000000000 ) ) ;
#2431 = VERTEX_POINT ( 'NONE', #14070 ) ;
#2432 = EDGE_CURVE ( 'NONE', #4388, #16762, #11119, .T. ) ;
#2433 = EDGE_CURVE ( 'NONE', #13613, #16356, #9943, .T. ) ;
#2434 = DIRECTION ( 'NONE',  ( -0.000000000000000000, 1.000000000000000000, -0.000000000000000000 ) ) ;
#2435 = ORIENTED_EDGE ( 'NONE', *, *, #17847, .T. ) ;
#2436 = DIRECTION ( 'NONE',  ( -1.000000000000000000, 0.000000000000000000, 0.000000000000000000 ) ) ;
#2437 = FACE_OUTER_BOUND ( 'NONE', #11871, .T. ) ;
#2438 = DIRECTION ( 'NONE',  ( 0.000000000000000000, -0.000000000000000000, 1.000000000000000000 ) ) ;
#2439 = EDGE_CURVE ( 'NONE', #7469, #17238, #5158, .T. ) ;
#2440 = CARTESIAN_POINT ( 'NONE',  ( 0.8561741729129472844, 61.93301270000000613, 46.60000000109246088 ) ) ;
#2441 = CARTESIAN_POINT ( 'NONE',  ( 13.00000000000000000, 2.055000000000000160, 0.000000000000000000 ) ) ;
#2442 = CARTESIAN_POINT ( 'NONE',  ( -41.00000000000000711, 110.0000000000000000, -30.99999999999999645 ) ) ;
#2443 = CARTESIAN_POINT ( 'NONE',  ( 1.976658868803501834, 62.97126298013989754, 45.00000000000001421 ) ) ;
#2444 = ORIENTED_EDGE ( 'NONE', *, *, #7937, .F. ) ;
#2445 = ORIENTED_EDGE ( 'NONE', *, *, #17190, .T. ) ;
#2446 = CARTESIAN_POINT ( 'NONE',  ( -14.83517299489740715, -16.99999999999997868, 4.263677507916957765 ) ) ;
#2447 = VECTOR ( 'NONE', #6633, 999.9999999999998863 ) ;
#2448 = DIRECTION ( 'NONE',  ( 0.000000000000000000, 0.000000000000000000, -1.000000000000000000 ) ) ;
#2449 = ORIENTED_EDGE ( 'NONE', *, *, #5921, .T. ) ;
#2450 = CARTESIAN_POINT ( 'NONE',  ( -15.16482700510263371, -18.99999999999997868, 42.98632249208304046 ) ) ;
#2451 = DIRECTION ( 'NONE',  ( -1.000000000000000000, -0.000000000000000000, -0.000000000000000000 ) ) ;
#2452 = EDGE_CURVE ( 'NONE', #4121, #15591, #10734, .T. ) ;
#2453 = ADVANCED_FACE ( 'NONE', ( #4872 ), #12405, .F. ) ;
#2454 = ORIENTED_EDGE ( 'NONE', *, *, #2913, .F. ) ;
#2455 = CARTESIAN_POINT ( 'NONE',  ( -18.04416526290808775, -23.36097942780924441, 26.14257249208303691 ) ) ;
#2456 = CARTESIAN_POINT ( 'NONE',  ( -41.00000000000000711, 53.00000000000000711, -5.000000000000000888 ) ) ;
#2457 = EDGE_LOOP ( 'NONE', ( #10247, #3332 ) ) ;
#2458 = LINE ( 'NONE', #8631, #14071 ) ;
#2459 = ORIENTED_EDGE ( 'NONE', *, *, #19083, .F. ) ;
#2460 = CARTESIAN_POINT ( 'NONE',  ( -25.00000000000000000, 110.0000000000000000, 30.00000000000000000 ) ) ;
#2461 = CARTESIAN_POINT ( 'NONE',  ( 34.99999999999999289, -6.000000000000000000, 42.49999999999997868 ) ) ;
#2462 = CIRCLE ( 'NONE', #15927, 5.800000000000007816 ) ;
#2463 = CARTESIAN_POINT ( 'NONE',  ( -41.00000000000000711, 53.00000000000000711, 20.00000000000000000 ) ) ;
#2464 = CARTESIAN_POINT ( 'NONE',  ( -17.64274437364855430, -28.24771351637087236, 33.57617750791696665 ) ) ;
#2465 = DIRECTION ( 'NONE',  ( 0.000000000000000000, -1.000000000000000000, -0.000000000000000000 ) ) ;
#2466 = CARTESIAN_POINT ( 'NONE',  ( -14.83517299489739649, -18.99999999999997868, 4.263677507916958653 ) ) ;
#2467 = VECTOR ( 'NONE', #5678, 1000.000000000000000 ) ;
#2468 = DIRECTION ( 'NONE',  ( 0.000000000000000000, 0.000000000000000000, 1.000000000000000000 ) ) ;
#2469 = VERTEX_POINT ( 'NONE', #16828 ) ;
#2470 = CARTESIAN_POINT ( 'NONE',  ( -22.04416526290809486, -22.28918265808477628, 26.14257249208303691 ) ) ;
#2471 = CARTESIAN_POINT ( 'NONE',  ( -9.999999999999994671, -24.16482700510257686, 37.07617750791695954 ) ) ;
#2472 = VECTOR ( 'NONE', #4112, 1000.000000000000000 ) ;
#2473 = EDGE_CURVE ( 'NONE', #3001, #7027, #9617, .T. ) ;
#2474 = CARTESIAN_POINT ( 'NONE',  ( 3.796994071234847710E-16, 61.93301269999999903, 48.15000000109247225 ) ) ;
#2475 = CARTESIAN_POINT ( 'NONE',  ( -11.46040770435014977, -20.21908421996103655, 38.39257249208301914 ) ) ;
#2476 = CARTESIAN_POINT ( 'NONE',  ( -2.066987300000001859, 64.85617417291294373, 44.70000000109248361 ) ) ;
#2477 = CARTESIAN_POINT ( 'NONE',  ( 1.035533905932739751, 61.50000000000000000, 46.35000000218494165 ) ) ;
#2478 = CARTESIAN_POINT ( 'NONE',  ( -9.955834737091912245, -22.82508104294696594, 26.35742750791695954 ) ) ;
#2479 = DIRECTION ( 'NONE',  ( -0.000000000000000000, 0.000000000000000000, 1.000000000000000000 ) ) ;
#2481 = CARTESIAN_POINT ( 'NONE',  ( -18.53959229564986799, -20.21908421996107563, 35.10742750791695244 ) ) ;
#2480 = VECTOR ( 'NONE', #2940, 1000.000000000000227 ) ;
#2482 = CARTESIAN_POINT ( 'NONE',  ( 2.499999999999999112, 65.03553390593273775, 46.55000000218494449 ) ) ;
#2483 = CARTESIAN_POINT ( 'NONE',  ( -10.75228648362912232, -21.35725562635138530, 38.61132249208304046 ) ) ;
#2484 = CARTESIAN_POINT ( 'NONE',  ( -1.035533905932738641, 66.50000000000000000, 49.04999999999999716 ) ) ;
#2485 = CARTESIAN_POINT ( 'NONE',  ( -5.800448837981397432, 29.77177811653248796, 56.71286850494549014 ) ) ;
#2486 = VECTOR ( 'NONE', #13156, 1000.000000000000000 ) ;
#2487 = AXIS2_PLACEMENT_3D ( 'NONE', #14795, #6951, #17439 ) ;
#2488 = CARTESIAN_POINT ( 'NONE',  ( -41.00000000000000711, 110.0000000000000000, 21.00000000000000000 ) ) ;
#2489 = CARTESIAN_POINT ( 'NONE',  ( -2.066987300000001415, 63.14382582708705627, 45.80000000109246372 ) ) ;
#2490 = CARTESIAN_POINT ( 'NONE',  ( -7.999999999999996447, -25.00000000000000711, 0.000000000000000000 ) ) ;
#2491 = ORIENTED_EDGE ( 'NONE', *, *, #26, .T. ) ;
#2492 = EDGE_CURVE ( 'NONE', #12636, #14875, #9834, .T. ) ;
#2493 = CARTESIAN_POINT ( 'NONE',  ( 3.796994071234847710E-16, 61.93301269999999903, 44.95000000109246940 ) ) ;
#2494 = CIRCLE ( 'NONE', #16609, 1.219500000000000028 ) ;
#2495 = EDGE_CURVE ( 'NONE', #2080, #15466, #3013, .T. ) ;
#2496 = CARTESIAN_POINT ( 'NONE',  ( -19.99999999999999645, -23.83517299489738051, 2.951177507916958209 ) ) ;
#2497 = LINE ( 'NONE', #8484, #1310 ) ;
#2498 = CARTESIAN_POINT ( 'NONE',  ( -8.855408670957602979, -27.35725562635137820, 34.23632249208304046 ) ) ;
#2499 = VECTOR ( 'NONE', #1288, 1000.000000000000000 ) ;
#2500 = CARTESIAN_POINT ( 'NONE',  ( -1.265664690411616068E-16, 66.06698730000000808, 49.55000000109247082 ) ) ;
#2501 = ORIENTED_EDGE ( 'NONE', *, *, #15791, .T. ) ;
#2502 = SHAPE_REPRESENTATION ( 'Browning Control Rotary Dial', ( #1791 ), #2636 ) ;
#2503 = DIRECTION ( 'NONE',  ( 0.000000000000000000, 0.7071067811865456854, 0.7071067811865494601 ) ) ;
#2504 = CARTESIAN_POINT ( 'NONE',  ( 7.500000000000005329, -38.00000000000000000, 4.500000000000000888 ) ) ;
#2505 = VECTOR ( 'NONE', #6895, 1000.000000000000000 ) ;
#2506 = CARTESIAN_POINT ( 'NONE',  ( 2.066987300000001415, 64.85617417291294373, 46.00000000109247367 ) ) ;
#2507 = DIRECTION ( 'NONE',  ( -8.177564888977974449E-17, -0.7071067811865495711, 0.7071067811865455743 ) ) ;
#2508 = CARTESIAN_POINT ( 'NONE',  ( -2.499999999999998668, 62.96446609406726225, 47.64999999999999858 ) ) ;
#2509 = AXIS2_PLACEMENT_3D ( 'NONE', #6095, #15302, #12353 ) ;
#2510 = CARTESIAN_POINT ( 'NONE',  ( -1.767766952966369765, 62.23223304703363112, 48.49999999999999289 ) ) ;
#2511 = AXIS2_PLACEMENT_3D ( 'NONE', #9422, #12649, #15416 ) ;
#2512 = CARTESIAN_POINT ( 'NONE',  ( -41.00000000000000711, 110.0000000000000000, 1.500000000000001332 ) ) ;
#2513 = ORIENTED_EDGE ( 'NONE', *, *, #12979, .T. ) ;
#2514 = ORIENTED_EDGE ( 'NONE', *, *, #632, .F. ) ;
#2515 = CARTESIAN_POINT ( 'NONE',  ( -12.95952864787948755, -30.95583473709188382, 3.392572492083039570 ) ) ;
#2516 = EDGE_CURVE ( 'NONE', #16874, #10684, #2394, .T. ) ;
#2517 = SURFACE_STYLE_USAGE ( .BOTH. , #9774 ) ;
#2518 = ORIENTED_EDGE ( 'NONE', *, *, #2101, .T. ) ;
#2519 = COLOUR_RGB ( '', 0.40784314, 0.44705882, 0.49803922) ;
#2521 = ORIENTED_EDGE ( 'NONE', *, *, #16911, .F. ) ;
#2520 = VERTEX_POINT ( 'NONE', #830 ) ;
#2522 = CARTESIAN_POINT ( 'NONE',  ( -18.04416526290808420, -24.63902057219074493, 7.982427507916962206 ) ) ;
#2523 = CARTESIAN_POINT ( 'NONE',  ( -20.97976432393977575, -20.35725562635143504, 34.88867750791695954 ) ) ;
#2524 = FACE_OUTER_BOUND ( 'NONE', #13829, .T. ) ;
#2525 = CARTESIAN_POINT ( 'NONE',  ( -2.500000000000000888, 62.96446609406726935, 46.95000000218495018 ) ) ;
#2526 = LINE ( 'NONE', #8412, #7509 ) ;
#2527 = ORIENTED_EDGE ( 'NONE', *, *, #2452, .T. ) ;
#2528 = EDGE_CURVE ( 'NONE', #3632, #7844, #3779, .T. ) ;
#2529 = VECTOR ( 'NONE', #8495, 1000.000000000000000 ) ;
#2530 = CARTESIAN_POINT ( 'NONE',  ( 2.500000000000001776, 64.00000000000000000, 49.99999999999999289 ) ) ;
#2531 = ORIENTED_EDGE ( 'NONE', *, *, #8652, .T. ) ;
#2532 = CARTESIAN_POINT ( 'NONE',  ( -47.00000000000001421, 30.87867965644036516, 42.87867965644034030 ) ) ;
#2533 = VERTEX_POINT ( 'NONE', #6812 ) ;
#2534 = CARTESIAN_POINT ( 'NONE',  ( 3.000000000000000000, 1.959434878635765477E-16, 1.600000000000000311 ) ) ;
#2535 = LINE ( 'NONE', #8517, #17195 ) ;
#2536 = CARTESIAN_POINT ( 'NONE',  ( 14.99999999999998579, 52.00000000000000711, 23.99999999999997158 ) ) ;
#2537 = CARTESIAN_POINT ( 'NONE',  ( 0.8561741729129460632, 66.06698729999999387, 46.10000000109246798 ) ) ;
#2538 = DIRECTION ( 'NONE',  ( 0.000000000000000000, 0.000000000000000000, -1.000000000000000000 ) ) ;
#2539 = VECTOR ( 'NONE', #4970, 1000.000000000000000 ) ;
#2540 = FACE_OUTER_BOUND ( 'NONE', #8912, .T. ) ;
#2541 = DIRECTION ( 'NONE',  ( -0.7071067811865463515, 0.000000000000000000, 0.7071067811865487940 ) ) ;
#2542 = ORIENTED_EDGE ( 'NONE', *, *, #17103, .F. ) ;
#2544 = ORIENTED_EDGE ( 'NONE', *, *, #706, .F. ) ;
#2543 = EDGE_LOOP ( 'NONE', ( #1272, #8187, #18133, #10701 ) ) ;
#2545 = CARTESIAN_POINT ( 'NONE',  ( -16.71081734191527346, -16.95583473709190159, 9.294927507916959541 ) ) ;
#2546 = VECTOR ( 'NONE', #1781, 1000.000000000000000 ) ;
#2547 = CARTESIAN_POINT ( 'NONE',  ( -41.00000000000000711, 53.00000000000000711, 26.50000000000000000 ) ) ;
#2548 = EDGE_LOOP ( 'NONE', ( #7155, #3668 ) ) ;
#2549 = EDGE_CURVE ( 'NONE', #5878, #3990, #9749, .T. ) ;
#2550 = CARTESIAN_POINT ( 'NONE',  ( -14.03132541760400009, -26.95583473709189448, 3.392572492083043567 ) ) ;
#2551 = EDGE_CURVE ( 'NONE', #10838, #14706, #8107, .T. ) ;
#2552 = CARTESIAN_POINT ( 'NONE',  ( 43.50000000000001421, 115.0000000000000000, 32.49999999999998579 ) ) ;
#2553 = ORIENTED_EDGE ( 'NONE', *, *, #18646, .F. ) ;
#2554 = CARTESIAN_POINT ( 'NONE',  ( -17.51566270880201159, -22.35725562635141728, 3.388677507916959986 ) ) ;
#2555 = CARTESIAN_POINT ( 'NONE',  ( 2.500000000000000000, 2.357898499370431722, -2.818925648462311528E-15 ) ) ;
#2556 = ORIENTED_EDGE ( 'NONE', *, *, #4085, .T. ) ;
#2557 = AXIS2_PLACEMENT_3D ( 'NONE', #116, #7461, #13432 ) ;
#2558 = CARTESIAN_POINT ( 'NONE',  ( -41.99999999999997868, 6.000000000000005329, -52.00000000000000000 ) ) ;
#2559 = VERTEX_POINT ( 'NONE', #7000 ) ;
#2560 = FACE_OUTER_BOUND ( 'NONE', #13945, .T. ) ;
#2561 = FACE_OUTER_BOUND ( 'NONE', #8300, .T. ) ;
#2562 = VECTOR ( 'NONE', #7706, 1000.000000000000000 ) ;
#2563 = CARTESIAN_POINT ( 'NONE',  ( -1.035533905932738863, 61.50000000000000000, 47.85000000218494165 ) ) ;
#2564 = CARTESIAN_POINT ( 'NONE',  ( -2.283493650000001818, 64.00000000000000000, 49.87500000054622973 ) ) ;
#2565 = CARTESIAN_POINT ( 'NONE',  ( -18.78091578003889950, -27.53959229564985378, 33.79492750791696665 ) ) ;
#2566 = DIRECTION ( 'NONE',  ( 1.000000000000000000, 1.156482317317871725E-16, -0.000000000000000000 ) ) ;
#2567 = CARTESIAN_POINT ( 'NONE',  ( -12.64274437364855252, -28.41254052147347053, 6.451177507916959541 ) ) ;
#2568 = DIRECTION ( 'NONE',  ( -0.8660254037844385966, 0.000000000000000000, 0.5000000000000001110 ) ) ;
#2569 = EDGE_CURVE ( 'NONE', #18998, #18134, #17590, .T. ) ;
#2570 = ORIENTED_EDGE ( 'NONE', *, *, #2199, .T. ) ;
#2571 = CARTESIAN_POINT ( 'NONE',  ( -10.04416526290808953, -22.49542703274172695, 7.330072492083041347 ) ) ;
#2572 = CARTESIAN_POINT ( 'NONE',  ( -20.97976432393977575, -20.35725562635143504, 8.638677507916955989 ) ) ;
#2573 = CARTESIAN_POINT ( 'NONE',  ( 2.066987300000001415, 64.00000000000000000, 48.35000000109246798 ) ) ;
#2574 = EDGE_CURVE ( 'NONE', #4107, #4659, #7190, .T. ) ;
#2575 = CARTESIAN_POINT ( 'NONE',  ( -20.04416526290809131, -22.82508104294699791, 36.64257249208304046 ) ) ;
#2576 = CARTESIAN_POINT ( 'NONE',  ( -0.8561741729129465073, 61.93301270000000613, 44.90000000109247225 ) ) ;
#2577 = ORIENTED_EDGE ( 'NONE', *, *, #528, .T. ) ;
#2578 = CARTESIAN_POINT ( 'NONE',  ( -2.315774708385926139, 31.32836399182264842, 54.80336399182263563 ) ) ;
#2579 = CARTESIAN_POINT ( 'NONE',  ( -13.82508104294698192, -29.04416526290806644, 32.91992750791695954 ) ) ;
#2580 = DIRECTION ( 'NONE',  ( 0.000000000000000000, 0.000000000000000000, 1.000000000000000000 ) ) ;
#2581 = CARTESIAN_POINT ( 'NONE',  ( -41.00000000000000711, 53.00000000000000711, 26.50000000000000000 ) ) ;
#2582 = CARTESIAN_POINT ( 'NONE',  ( -40.00000000000000711, 110.0000000000000000, -19.00000000000000355 ) ) ;
#2583 = CARTESIAN_POINT ( 'NONE',  ( -13.82508104294702100, -18.95583473709188382, 37.95507249208304046 ) ) ;
#2584 = CARTESIAN_POINT ( 'NONE',  ( 1.035533905932738197, 66.50000000000000000, 46.54999999999999716 ) ) ;
#2585 = DIRECTION ( 'NONE',  ( -0.000000000000000000, -1.000000000000000000, -0.000000000000000000 ) ) ;
#2586 = ADVANCED_FACE ( 'NONE', ( #1026 ), #15741, .F. ) ;
#2587 = CARTESIAN_POINT ( 'NONE',  ( -32.50000000000000000, 53.00000000000000711, 15.00000000000000000 ) ) ;
#2588 = CARTESIAN_POINT ( 'NONE',  ( 0.8561741729129472844, 61.93301270000000613, 46.00000000109245946 ) ) ;
#2589 = CARTESIAN_POINT ( 'NONE',  ( -0.000000000000000000, -32.00000000000000711, 0.000000000000000000 ) ) ;
#2590 = VERTEX_POINT ( 'NONE', #4167 ) ;
#2591 = FILL_AREA_STYLE ('',( #1523 ) ) ;
#2592 = CARTESIAN_POINT ( 'NONE',  ( 2.066987300000001859, 63.14382582708704916, 45.10000000109246798 ) ) ;
#2593 = CARTESIAN_POINT ( 'NONE',  ( -9.955834737091912245, -22.82508104294696594, 5.357427507916956877 ) ) ;
#2594 = EDGE_CURVE ( 'NONE', #11453, #15669, #18162, .T. ) ;
#2595 = DIRECTION ( 'NONE',  ( -0.000000000000000000, -1.000000000000000000, -0.000000000000000000 ) ) ;
#2596 = CARTESIAN_POINT ( 'NONE',  ( -9.020235676060250896, -20.35725562635137820, 33.36132249208304046 ) ) ;
#2597 = CARTESIAN_POINT ( 'NONE',  ( 2.066987300000001859, 64.85617417291294373, 48.60000000109246798 ) ) ;
#2598 = CARTESIAN_POINT ( 'NONE',  ( -15.96867458239597326, -26.95583473709190159, 33.35742750791695954 ) ) ;
#2599 = CARTESIAN_POINT ( 'NONE',  ( -17.35725562635144215, -19.58745947852648683, 3.826177507916958209 ) ) ;
#2600 = LINE ( 'NONE', #12704, #11302 ) ;
#2601 = CARTESIAN_POINT ( 'NONE',  ( -2.066987300000000971, 63.14382582708704916, 45.60000000109246798 ) ) ;
#2602 = CARTESIAN_POINT ( 'NONE',  ( -50.00000000000002132, 33.00000000000000000, 44.99999999999999289 ) ) ;
#2603 = DIRECTION ( 'NONE',  ( 0.000000000000000000, 0.000000000000000000, 1.000000000000000000 ) ) ;
#2604 = CARTESIAN_POINT ( 'NONE',  ( 5.421010862427523748E-15, -25.00000000000000711, 1.500000000000000000 ) ) ;
#2605 = CARTESIAN_POINT ( 'NONE',  ( -40.00000000000000711, 110.0000000000000000, 30.00000000000000000 ) ) ;
#2606 = ORIENTED_EDGE ( 'NONE', *, *, #1150, .T. ) ;
#2607 = ORIENTED_EDGE ( 'NONE', *, *, #14511, .T. ) ;
#2608 = CARTESIAN_POINT ( 'NONE',  ( -9.020235676060250896, -20.35725562635137820, 1.861322492083039126 ) ) ;
#2609 = VERTEX_POINT ( 'NONE', #17007 ) ;
#2611 = ORIENTED_EDGE ( 'NONE', *, *, #569, .F. ) ;
#2610 = ORIENTED_EDGE ( 'NONE', *, *, #17643, .F. ) ;
#2612 = CARTESIAN_POINT ( 'NONE',  ( -15.96867458239597326, -26.95583473709190159, 7.107427507916960430 ) ) ;
#2613 = CARTESIAN_POINT ( 'NONE',  ( -21.14459132904236327, -27.35725562635143149, 28.76367750791696309 ) ) ;
#2614 = FACE_OUTER_BOUND ( 'NONE', #16515, .T. ) ;
#2615 = CARTESIAN_POINT ( 'NONE',  ( 0.8561741729129472844, 61.93301270000000613, 48.20000000109248361 ) ) ;
#2616 = CARTESIAN_POINT ( 'NONE',  ( 49.99999999999997868, 32.99999999999999289, 45.00000000000000000 ) ) ;
#2617 = ORIENTED_EDGE ( 'NONE', *, *, #13137, .F. ) ;
#2618 = CARTESIAN_POINT ( 'NONE',  ( 0.000000000000000000, 3.000000000000000000, -52.00000000000000000 ) ) ;
#2619 = EDGE_LOOP ( 'NONE', ( #13810, #16935, #15387, #13295 ) ) ;
#2621 = DIRECTION ( 'NONE',  ( -0.000000000000000000, -0.000000000000000000, -1.000000000000000000 ) ) ;
#2620 = AXIS2_PLACEMENT_3D ( 'NONE', #809, #2566, #7074 ) ;
#2622 = EDGE_LOOP ( 'NONE', ( #14006, #10142 ) ) ;
#2623 = DIRECTION ( 'NONE',  ( 9.440833060721746417E-33, 1.000000000000000000, 1.632680918566406793E-16 ) ) ;
#2624 = LINE ( 'NONE', #2349, #10921 ) ;
#2625 = CARTESIAN_POINT ( 'NONE',  ( -41.00000000000000711, 53.00000000000000711, -30.99999999999999645 ) ) ;
#2626 = CARTESIAN_POINT ( 'NONE',  ( 2.066987300000001859, 64.85617417291294373, 45.20000000109248361 ) ) ;
#2627 = FACE_OUTER_BOUND ( 'NONE', #3409, .T. ) ;
#2628 = CARTESIAN_POINT ( 'NONE',  ( 4.592425496802577917E-16, 61.50000000000000000, 47.10000000218494165 ) ) ;
#2629 = DIRECTION ( 'NONE',  ( -8.163404592832032733E-17, 0.000000000000000000, -1.000000000000000000 ) ) ;
#2630 = EDGE_LOOP ( 'NONE', ( #10961, #6937, #15456, #10655 ) ) ;
#2632 = EDGE_LOOP ( 'NONE', ( #9083, #4504, #1768, #9775 ) ) ;
#2631 = VERTEX_POINT ( 'NONE', #9536 ) ;
#2633 = ADVANCED_FACE ( 'NONE', ( #619, #11006, #15527, #13754, #10714, #3373, #4762 ), #12184, .F. ) ;
#2635 = EDGE_CURVE ( 'NONE', #9275, #12801, #2195, .T. ) ;
#2634 = CARTESIAN_POINT ( 'NONE',  ( -14.83517299489739649, -18.99999999999997868, 41.01367750791696665 ) ) ;
#2636 =( GEOMETRIC_REPRESENTATION_CONTEXT ( 3 ) GLOBAL_UNCERTAINTY_ASSIGNED_CONTEXT ( ( #16291 ) ) GLOBAL_UNIT_ASSIGNED_CONTEXT ( ( #11213, #5357, #8294 ) ) REPRESENTATION_CONTEXT ( 'NONE', 'WORKASPACE' ) );
#2637 = DIRECTION ( 'NONE',  ( 0.000000000000000000, -1.000000000000000000, 0.000000000000000000 ) ) ;
#2638 = ORIENTED_EDGE ( 'NONE', *, *, #16555, .F. ) ;
#2639 = VECTOR ( 'NONE', #11984, 1000.000000000000000 ) ;
#2640 = CARTESIAN_POINT ( 'NONE',  ( -18.78091578003892081, -20.46040770435013556, 42.33007249208301914 ) ) ;
#2641 = EDGE_CURVE ( 'NONE', #13312, #18550, #10633, .T. ) ;
#2642 = DIRECTION ( 'NONE',  ( -0.000000000000000000, -0.000000000000000000, -1.000000000000000000 ) ) ;
#2643 = ORIENTED_EDGE ( 'NONE', *, *, #848, .T. ) ;
#2644 = CARTESIAN_POINT ( 'NONE',  ( -17.51566270880201159, -22.35725562635141728, 8.638677507916959541 ) ) ;
#2645 = EDGE_CURVE ( 'NONE', #677, #16168, #16710, .T. ) ;
#2646 = SURFACE_SIDE_STYLE ('',( #4135 ) ) ;
#2647 = ORIENTED_EDGE ( 'NONE', *, *, #8995, .F. ) ;
#2648 = DIRECTION ( 'NONE',  ( -2.665111688417744333E-15, -1.000000000000000000, 0.000000000000000000 ) ) ;
#2649 = ORIENTED_EDGE ( 'NONE', *, *, #17189, .T. ) ;
#2650 = DIRECTION ( 'NONE',  ( 1.000000000000000000, 0.000000000000000000, 0.000000000000000000 ) ) ;
#2651 = DIRECTION ( 'NONE',  ( -0.000000000000000000, -0.000000000000000000, -1.000000000000000000 ) ) ;
#2652 = AXIS2_PLACEMENT_3D ( 'NONE', #6033, #6129, #11993 ) ;
#2653 = CARTESIAN_POINT ( 'NONE',  ( 12.99999999999999822, 2.789133085058097101E-16, -2.055000000000000160 ) ) ;
#2654 = AXIS2_PLACEMENT_3D ( 'NONE', #5320, #4141, #13134 ) ;
#2655 = PRODUCT_CONTEXT ( 'NONE', #1429, 'mechanical' ) ;
#2656 = DIRECTION ( 'NONE',  ( -1.000000000000000000, 0.000000000000000000, -0.000000000000000000 ) ) ;
#2657 = EDGE_CURVE ( 'NONE', #895, #7943, #12290, .T. ) ;
#2658 = CARTESIAN_POINT ( 'NONE',  ( -16.50457296725820555, -28.95583473709189448, 28.10742750791695954 ) ) ;
#2659 = FACE_BOUND ( 'NONE', #11637, .T. ) ;
#2660 = CARTESIAN_POINT ( 'NONE',  ( 5.199999999999996625, 0.000000000000000000, 0.000000000000000000 ) ) ;
#2661 = CARTESIAN_POINT ( 'NONE',  ( 11.83926609531033058, -43.78611686177728046, 1.500000000000000000 ) ) ;
#2662 = ORIENTED_EDGE ( 'NONE', *, *, #15902, .T. ) ;
#2663 = ADVANCED_FACE ( 'NONE', ( #6513 ), #18184, .T. ) ;
#2664 = CARTESIAN_POINT ( 'NONE',  ( -21.14459132904239169, -20.64274437364858628, 42.11132249208304046 ) ) ;
#2665 = VECTOR ( 'NONE', #8253, 1000.000000000000000 ) ;
#2666 = CARTESIAN_POINT ( 'NONE',  ( -17.64274437364855430, -28.24771351637087236, 38.82617750791695954 ) ) ;
#2667 = VECTOR ( 'NONE', #16932, 1000.000000000000000 ) ;
#2668 = CARTESIAN_POINT ( 'NONE',  ( -2.066987300000001415, 63.14382582708705627, 48.80000000109247082 ) ) ;
#2669 = CARTESIAN_POINT ( 'NONE',  ( -13.64274437364857739, -21.31951028609534760, 1.423822492083042901 ) ) ;
#2670 = VERTEX_POINT ( 'NONE', #9248 ) ;
#2671 = DIRECTION ( 'NONE',  ( -0.000000000000000000, -1.000000000000000000, -0.000000000000000000 ) ) ;
#2672 = CARTESIAN_POINT ( 'NONE',  ( 4.160453206537142457, 32.60057016663802187, 53.88344170207938788 ) ) ;
#2673 = DIRECTION ( 'NONE',  ( 0.000000000000000000, 0.000000000000000000, -1.000000000000000000 ) ) ;
#2674 = CARTESIAN_POINT ( 'NONE',  ( -19.99999999999999645, -23.83517299489738051, 39.70117750791695954 ) ) ;
#2675 = PLANE ( 'NONE',  #9957 ) ;
#2676 = CARTESIAN_POINT ( 'NONE',  ( -11.21908421996106142, -27.53959229564982181, 34.45507249208304046 ) ) ;
#2677 = EDGE_CURVE ( 'NONE', #19215, #11338, #6321, .T. ) ;
#2678 = EDGE_CURVE ( 'NONE', #11126, #18238, #17229, .T. ) ;
#2679 = APPLICATION_CONTEXT ( 'automotive_design' ) ;
#2680 = CARTESIAN_POINT ( 'NONE',  ( 2.500000000000002220, 62.96446609406726935, 47.14999999999999858 ) ) ;
#2681 = DIRECTION ( 'NONE',  ( 0.000000000000000000, 0.000000000000000000, -1.000000000000000000 ) ) ;
#2682 = EDGE_CURVE ( 'NONE', #14781, #19196, #15328, .T. ) ;
#2683 = VECTOR ( 'NONE', #14243, 1000.000000000000000 ) ;
#2684 = VECTOR ( 'NONE', #17099, 1000.000000000000000 ) ;
#2685 = PRODUCT_DEFINITION_SHAPE ( 'NONE', 'NONE',  #9182 ) ;
#2686 = CARTESIAN_POINT ( 'NONE',  ( 1.767766952966370653, 62.23223304703363112, 48.80000000218494449 ) ) ;
#2687 = EDGE_CURVE ( 'NONE', #16539, #2590, #5044, .T. ) ;
#2688 = CARTESIAN_POINT ( 'NONE',  ( -1.767766952966369765, 62.23223304703363112, 45.29999999999999005 ) ) ;
#2689 = DIRECTION ( 'NONE',  ( -1.000000000000000000, -0.000000000000000000, -0.000000000000000000 ) ) ;
#2690 = VERTEX_POINT ( 'NONE', #7653 ) ;
#2691 = CARTESIAN_POINT ( 'NONE',  ( -16.17491895705301275, -18.95583473709189803, 9.294927507916954212 ) ) ;
#2692 = CARTESIAN_POINT ( 'NONE',  ( -18.04416526290808420, -24.63902057219074493, 39.48242750791696665 ) ) ;
#2693 = DIRECTION ( 'NONE',  ( -0.7071067811865463515, 0.5000000000000024425, -0.4999999999999993339 ) ) ;
#2694 = CARTESIAN_POINT ( 'NONE',  ( -15.16482700510263371, -18.99999999999997868, 6.236322492083041347 ) ) ;
#2695 = CIRCLE ( 'NONE', #18053, 4.000000000000001776 ) ;
#2696 = CONICAL_SURFACE ( 'NONE', #13654, 5.800000000000005151, 0.7853981633974385090 ) ;
#2697 = CARTESIAN_POINT ( 'NONE',  ( -0.8561741729129461742, 66.06698729999999387, 49.60000000109246798 ) ) ;
#2698 = EDGE_CURVE ( 'NONE', #15286, #14415, #16572, .T. ) ;
#2699 = CARTESIAN_POINT ( 'NONE',  ( -12.31951028609537602, -22.64274437364854364, 31.38867750791696309 ) ) ;
#2700 = LINE ( 'NONE', #10432, #10637 ) ;
#2701 = DIRECTION ( 'NONE',  ( -0.000000000000000000, -0.7071067811865456854, -0.7071067811865494601 ) ) ;
#2702 = DIRECTION ( 'NONE',  ( -1.000000000000000000, -0.000000000000000000, -0.000000000000000000 ) ) ;
#2703 = CARTESIAN_POINT ( 'NONE',  ( -37.50000000000002132, -6.000000000000000000, 47.49999999999997868 ) ) ;
#2704 = CARTESIAN_POINT ( 'NONE',  ( 2.750000000000009770, 38.00000000000000000, 40.49999999999995737 ) ) ;
#2705 = CARTESIAN_POINT ( 'NONE',  ( 2.066987300000001415, 64.00000000000000000, 46.95000000109246940 ) ) ;
#2706 = DIRECTION ( 'NONE',  ( 0.7071067811865487940, 1.226634733346701480E-15, 0.7071067811865462405 ) ) ;
#2707 =( GEOMETRIC_REPRESENTATION_CONTEXT ( 3 ) GLOBAL_UNCERTAINTY_ASSIGNED_CONTEXT ( ( #16714 ) ) GLOBAL_UNIT_ASSIGNED_CONTEXT ( ( #12339, #6186, #18241 ) ) REPRESENTATION_CONTEXT ( 'NONE', 'WORKASPACE' ) );
#2708 = VECTOR ( 'NONE', #14350, 1000.000000000000000 ) ;
#2709 = LINE ( 'NONE', #10442, #9883 ) ;
#2710 = ORIENTED_EDGE ( 'NONE', *, *, #11748, .T. ) ;
#2711 = ORIENTED_EDGE ( 'NONE', *, *, #9387, .F. ) ;
#2712 = CARTESIAN_POINT ( 'NONE',  ( -21.14459132904239169, -20.64274437364858628, 5.361322492083039570 ) ) ;
#2713 =( LENGTH_UNIT ( ) NAMED_UNIT ( * ) SI_UNIT ( .MILLI., .METRE. ) );
#2714 = VERTEX_POINT ( 'NONE', #8917 ) ;
#2715 = CARTESIAN_POINT ( 'NONE',  ( -11.46040770435015332, -20.21908421996104011, 1.642572492083041125 ) ) ;
#2717 = ORIENTED_EDGE ( 'NONE', *, *, #8293, .T. ) ;
#2716 = ORIENTED_EDGE ( 'NONE', *, *, #164, .T. ) ;
#2718 = CARTESIAN_POINT ( 'NONE',  ( -17.99999999999999645, -23.83517299489736985, 2.951177507916960430 ) ) ;
#2719 = CARTESIAN_POINT ( 'NONE',  ( -9.996306089212364299, -29.24501739517662813, 37.73242750791695244 ) ) ;
#2720 = DIRECTION ( 'NONE',  ( -0.000000000000000000, -1.000000000000000000, -0.000000000000000000 ) ) ;
#2721 = CARTESIAN_POINT ( 'NONE',  ( -1.767766952966369765, 62.23223304703363112, 45.40000000218494591 ) ) ;
#2722 = CARTESIAN_POINT ( 'NONE',  ( -32.50000000000000000, 53.00000000000000711, 17.64999999999998437 ) ) ;
#2723 = ADVANCED_FACE ( 'NONE', ( #16272 ), #1579, .F. ) ;
#2724 = EDGE_LOOP ( 'NONE', ( #13146, #2369 ) ) ;
#2725 =( GEOMETRIC_REPRESENTATION_CONTEXT ( 3 ) GLOBAL_UNCERTAINTY_ASSIGNED_CONTEXT ( ( #5516 ) ) GLOBAL_UNIT_ASSIGNED_CONTEXT ( ( #2713, #5857, #7224 ) ) REPRESENTATION_CONTEXT ( 'NONE', 'WORKASPACE' ) );
#2726 = CARTESIAN_POINT ( 'NONE',  ( -32.50000000000001421, -6.000000000000000000, 24.99999999999998224 ) ) ;
#2727 = ORIENTED_EDGE ( 'NONE', *, *, #7372, .T. ) ;
#2728 = ORIENTED_EDGE ( 'NONE', *, *, #1850, .F. ) ;
#2729 = CARTESIAN_POINT ( 'NONE',  ( -9.551088096457694952E-15, 22.67157287525377996, 59.57106781186547551 ) ) ;
#2730 = CARTESIAN_POINT ( 'NONE',  ( -0.1250000000000104083, 27.16170093578836031, 58.97002704785691662 ) ) ;
#2731 = DIRECTION ( 'NONE',  ( -0.7071067811865335839, 8.659560562355102956E-17, -0.7071067811865614505 ) ) ;
#2732 = CARTESIAN_POINT ( 'NONE',  ( -2.066987300000001415, 64.00000000000000000, 49.75000000109246656 ) ) ;
#2733 = CARTESIAN_POINT ( 'NONE',  ( -4.744034285469996171, -45.28611686177728046, 1.500000000000000000 ) ) ;
#2734 = LINE ( 'NONE', #878, #17090 ) ;
#2735 = DIRECTION ( 'NONE',  ( 0.000000000000000000, 0.000000000000000000, -1.000000000000000000 ) ) ;
#2736 = VERTEX_POINT ( 'NONE', #1379 ) ;
#2738 = ORIENTED_EDGE ( 'NONE', *, *, #11216, .F. ) ;
#2737 = ORIENTED_EDGE ( 'NONE', *, *, #8879, .T. ) ;
#2739 = CARTESIAN_POINT ( 'NONE',  ( -20.24501739517664234, -29.00369391078761439, 7.544927507916956877 ) ) ;
#2740 =( BOUNDED_CURVE ( )  B_SPLINE_CURVE ( 2, ( #11887, #17884, #13255, #10411, #19254, #2970, #14123, #3441, #2161 ),
 .UNSPECIFIED., .F., .F. ) 
 B_SPLINE_CURVE_WITH_KNOTS ( ( 3, 2, 2, 2, 3 ),
 ( 0.7857142857142856984, 0.8035714285714286031, 0.8214285714285713969, 0.8392857142857141906, 0.8571428571428569843 ),
 .UNSPECIFIED. ) 
 CURVE ( )  GEOMETRIC_REPRESENTATION_ITEM ( )  RATIONAL_B_SPLINE_CURVE ( ( 1.000000000000000000, 0.9238795325112867385, 1.000000000000000000, 0.9238795325112867385, 1.000000000000000000, 0.9238795325112867385, 1.000000000000000000, 0.9238795325112871826, 0.9999999999999995559 ) ) 
 REPRESENTATION_ITEM ( '' )  );
#2741 = ORIENTED_EDGE ( 'NONE', *, *, #4371, .F. ) ;
#2742 = ORIENTED_EDGE ( 'NONE', *, *, #16837, .F. ) ;
#2743 = CARTESIAN_POINT ( 'NONE',  ( -9.999999999999994671, -23.83517299489734143, 39.04882249208304046 ) ) ;
#2744 = LINE ( 'NONE', #11847, #15946 ) ;
#2745 = ORIENTED_EDGE ( 'NONE', *, *, #2099, .F. ) ;
#2746 = CARTESIAN_POINT ( 'NONE',  ( -12.68318583509884157, -21.92450931948787485, -0.3300724920830400699 ) ) ;
#2747 = LINE ( 'NONE', #16276, #10025 ) ;
#2748 = ORIENTED_EDGE ( 'NONE', *, *, #7353, .T. ) ;
#2749 = DIRECTION ( 'NONE',  ( 0.000000000000000000, 0.7071067811865492381, -0.7071067811865457964 ) ) ;
#2750 = ORIENTED_EDGE ( 'NONE', *, *, #7416, .T. ) ;
#2751 = DIRECTION ( 'NONE',  ( 0.000000000000000000, 0.000000000000000000, 1.000000000000000000 ) ) ;
#2752 = CARTESIAN_POINT ( 'NONE',  ( -25.00000000000001421, -6.000000000000000000, 47.49999999999997868 ) ) ;
#2753 = LINE ( 'NONE', #1000, #7231 ) ;
#2754 = PLANE ( 'NONE',  #12879 ) ;
#2755 = CARTESIAN_POINT ( 'NONE',  ( -10.58745947852649927, -21.64274437364853654, 20.88867750791695954 ) ) ;
#2756 = CARTESIAN_POINT ( 'NONE',  ( 11.83926609531033058, -43.78611686177728046, 3.000000000000000000 ) ) ;
#2758 = EDGE_CURVE ( 'NONE', #15605, #18409, #18146, .T. ) ;
#2757 = CARTESIAN_POINT ( 'NONE',  ( -13.49542703274178379, -19.04416526290806289, 4.482427507916957765 ) ) ;
#2759 = DIRECTION ( 'NONE',  ( -1.000000000000000000, -0.000000000000000000, -0.000000000000000000 ) ) ;
#2760 = ORIENTED_EDGE ( 'NONE', *, *, #18994, .F. ) ;
#2761 = UNCERTAINTY_MEASURE_WITH_UNIT (LENGTH_MEASURE( 1.000000000000000082E-05 ), #4144, 'distance_accuracy_value', 'NONE');
#2762 = CARTESIAN_POINT ( 'NONE',  ( -20.04416526290809131, -22.82508104294699791, 5.142572492083038682 ) ) ;
#2763 = CARTESIAN_POINT ( 'NONE',  ( -11.35725562635144925, -18.02023567606020293, 9.951177507916955989 ) ) ;
#2764 = CARTESIAN_POINT ( 'NONE',  ( 3.796994071234847710E-16, 61.93301269999999903, 44.95000000109246940 ) ) ;
#2765 = CARTESIAN_POINT ( 'NONE',  ( -18.53959229564982536, -27.78091578003890660, 41.01757249208304046 ) ) ;
#2766 = AXIS2_PLACEMENT_3D ( 'NONE', #14766, #1435, #3200 ) ;
#2767 = DIRECTION ( 'NONE',  ( 0.7071067811865512365, 0.4999999999999988898, -0.4999999999999959477 ) ) ;
#2768 = ORIENTED_EDGE ( 'NONE', *, *, #18009, .F. ) ;
#2769 = DIRECTION ( 'NONE',  ( 0.000000000000000000, -0.7071067811865454633, -0.7071067811865496822 ) ) ;
#2770 = FACE_OUTER_BOUND ( 'NONE', #13066, .T. ) ;
#2771 = EDGE_CURVE ( 'NONE', #13230, #16897, #9705, .T. ) ;
#2772 = PLANE ( 'NONE',  #13601 ) ;
#2773 = CARTESIAN_POINT ( 'NONE',  ( -32.50000000000000000, 47.00000000000000711, -32.50000000000000000 ) ) ;
#2774 = CARTESIAN_POINT ( 'NONE',  ( 0.1249999999999895917, 25.46464466094064250, 60.66708332270462734 ) ) ;
#2775 = CARTESIAN_POINT ( 'NONE',  ( -14.83517299489735741, -28.99999999999998224, 40.36132249208304046 ) ) ;
#2776 = CARTESIAN_POINT ( 'NONE',  ( 2.500000000000002220, 62.96446609406726935, 47.94999999999999574 ) ) ;
#2777 = CARTESIAN_POINT ( 'NONE',  ( 2.066987300000001415, 64.85617417291294373, 47.80000000109247082 ) ) ;
#2778 = AXIS2_PLACEMENT_3D ( 'NONE', #6950, #9698, #15784 ) ;
#2779 = CARTESIAN_POINT ( 'NONE',  ( -2.500000000000001776, 65.03553390593273775, 46.74999999999999289 ) ) ;
#2780 = CARTESIAN_POINT ( 'NONE',  ( 1.035533905932739751, 61.50000000000000000, 46.24999999999998579 ) ) ;
#2781 = CARTESIAN_POINT ( 'NONE',  ( -5.799326430397249155, 29.83055285973289372, 56.65377616443620212 ) ) ;
#2782 = VECTOR ( 'NONE', #4479, 1000.000000000000000 ) ;
#2783 = ORIENTED_EDGE ( 'NONE', *, *, #19177, .T. ) ;
#2784 = EDGE_CURVE ( 'NONE', #4943, #18801, #6593, .T. ) ;
#2785 = CARTESIAN_POINT ( 'NONE',  ( -11.21908421996108629, -20.46040770435011069, -0.3300724920830416798 ) ) ;
#2786 = EDGE_CURVE ( 'NONE', #18046, #15953, #15628, .T. ) ;
#2787 = CARTESIAN_POINT ( 'NONE',  ( -16.17491895705301275, -18.95583473709189803, 14.54492750791695421 ) ) ;
#2788 = FACE_OUTER_BOUND ( 'NONE', #6329, .T. ) ;
#2789 = ADVANCED_FACE ( 'NONE', ( #1772 ), #11848, .T. ) ;
#2790 = CARTESIAN_POINT ( 'NONE',  ( -13.82508104294702100, -18.95583473709188382, 11.70507249208303868 ) ) ;
#2791 = AXIS2_PLACEMENT_3D ( 'NONE', #16606, #9441, #615 ) ;
#2792 = CARTESIAN_POINT ( 'NONE',  ( -2.066987300000001415, 63.14382582708705627, 44.80000000109247082 ) ) ;
#2793 = CARTESIAN_POINT ( 'NONE',  ( -11.21908421996108629, -20.46040770435011069, 4.919927507916955989 ) ) ;
#2794 = CARTESIAN_POINT ( 'NONE',  ( -11.21908421996108984, -20.46040770435011069, 4.919927507916956877 ) ) ;
#2795 = AXIS2_PLACEMENT_3D ( 'NONE', #1994, #15521, #13948 ) ;
#2796 = LINE ( 'NONE', #7209, #15707 ) ;
#2797 = VECTOR ( 'NONE', #5397, 1000.000000000000000 ) ;
#2798 = CARTESIAN_POINT ( 'NONE',  ( -41.00000000000000711, 110.0000000000000000, 1.500000000000001332 ) ) ;
#2799 = DIRECTION ( 'NONE',  ( 0.000000000000000000, 0.000000000000000000, 1.000000000000000000 ) ) ;
#2800 = DIRECTION ( 'NONE',  ( -1.000000000000000000, 0.000000000000000000, 0.000000000000000000 ) ) ;
#2801 = VECTOR ( 'NONE', #7551, 1000.000000000000000 ) ;
#2802 = CARTESIAN_POINT ( 'NONE',  ( -1.461580736456473906, 65.46158073645646880, 48.85000000109246798 ) ) ;
#2803 = PLANE ( 'NONE',  #5988 ) ;
#2804 = AXIS2_PLACEMENT_3D ( 'NONE', #7067, #5319, #17280 ) ;
#2805 = DIRECTION ( 'NONE',  ( 0.000000000000000000, 0.000000000000000000, -1.000000000000000000 ) ) ;
#2806 = ORIENTED_EDGE ( 'NONE', *, *, #19318, .F. ) ;
#2807 = ORIENTED_EDGE ( 'NONE', *, *, #9847, .T. ) ;
#2808 = CARTESIAN_POINT ( 'NONE',  ( -18.35725562635138886, -30.14459132904237393, 14.54882249208303868 ) ) ;
#2809 = VECTOR ( 'NONE', #18445, 1000.000000000000000 ) ;
#2810 = EDGE_CURVE ( 'NONE', #16642, #6640, #12148, .T. ) ;
#2811 = CARTESIAN_POINT ( 'NONE',  ( -9.971658890789427512E-15, 29.83102903476757817, 56.65425233947097894 ) ) ;
#2813 = ORIENTED_EDGE ( 'NONE', *, *, #2492, .F. ) ;
#2812 = ORIENTED_EDGE ( 'NONE', *, *, #3312, .T. ) ;
#2814 = CARTESIAN_POINT ( 'NONE',  ( -13.35725562635142794, -21.48433729119796709, -0.5488224920830401254 ) ) ;
#2815 = CARTESIAN_POINT ( 'NONE',  ( -13.28918265808478694, -16.95583473709189093, 6.455072492083038682 ) ) ;
#2816 = AXIS2_PLACEMENT_3D ( 'NONE', #12177, #127, #12077 ) ;
#2817 = CARTESIAN_POINT ( 'NONE',  ( 44.99999999999997158, 3.000000000000000000, 55.00000000000000000 ) ) ;
#2818 = CARTESIAN_POINT ( 'NONE',  ( -2.500000000000001776, 65.03553390593273775, 46.05000000218494449 ) ) ;
#2819 = ORIENTED_EDGE ( 'NONE', *, *, #8356, .F. ) ;
#2820 = ORIENTED_EDGE ( 'NONE', *, *, #36, .F. ) ;
#2821 = PLANE ( 'NONE',  #15385 ) ;
#2822 = ORIENTED_EDGE ( 'NONE', *, *, #14511, .F. ) ;
#2823 = ORIENTED_EDGE ( 'NONE', *, *, #14262, .F. ) ;
#2824 = CARTESIAN_POINT ( 'NONE',  ( 1.767766952966369987, 65.76776695296638309, 45.69999999999999574 ) ) ;
#2825 = DIRECTION ( 'NONE',  ( 0.000000000000000000, -0.7071067811865497932, 0.7071067811865452413 ) ) ;
#2826 = DIRECTION ( 'NONE',  ( 0.000000000000000000, -0.7071067811865454633, -0.7071067811865496822 ) ) ;
#2827 = CONICAL_SURFACE ( 'NONE', #3142, 1.219500000000000028, 0.7853981633974680410 ) ;
#2828 = CARTESIAN_POINT ( 'NONE',  ( 0.8561741729129472844, 61.93301270000000613, 47.60000000109246798 ) ) ;
#2829 = CARTESIAN_POINT ( 'NONE',  ( -15.00000000000000000, -37.50000000000000000, 7.999999999999996447 ) ) ;
#2830 =( GEOMETRIC_REPRESENTATION_CONTEXT ( 3 ) GLOBAL_UNCERTAINTY_ASSIGNED_CONTEXT ( ( #12586 ) ) GLOBAL_UNIT_ASSIGNED_CONTEXT ( ( #3654, #9623, #17088 ) ) REPRESENTATION_CONTEXT ( 'NONE', 'WORKASPACE' ) );
#2831 = DIRECTION ( 'NONE',  ( -0.000000000000000000, -0.000000000000000000, -1.000000000000000000 ) ) ;
#2832 = EDGE_CURVE ( 'NONE', #1370, #6673, #7755, .T. ) ;
#2833 = ORIENTED_EDGE ( 'NONE', *, *, #14108, .F. ) ;
#2835 = VERTEX_POINT ( 'NONE', #17850 ) ;
#2834 = EDGE_LOOP ( 'NONE', ( #955, #34 ) ) ;
#2836 = CARTESIAN_POINT ( 'NONE',  ( -9.996306089212364299, -29.24501739517662813, 0.9824275079169565439 ) ) ;
#2837 = DIRECTION ( 'NONE',  ( 0.000000000000000000, 0.000000000000000000, -1.000000000000000000 ) ) ;
#2838 = CIRCLE ( 'NONE', #1593, 2.750000000000000000 ) ;
#2839 = ORIENTED_EDGE ( 'NONE', *, *, #18941, .T. ) ;
#2840 = ORIENTED_EDGE ( 'NONE', *, *, #138, .F. ) ;
#2841 = CARTESIAN_POINT ( 'NONE',  ( -17.64274437364858983, -19.75228648362910633, 42.54882249208304046 ) ) ;
#2842 = CARTESIAN_POINT ( 'NONE',  ( 46.99999999999997868, 118.0000000000000142, 37.49999999999997868 ) ) ;
#2843 = CARTESIAN_POINT ( 'NONE',  ( -24.00000000000000000, 53.00000000000000711, 21.00000000000000000 ) ) ;
#2844 = ADVANCED_FACE ( 'NONE', ( #3041 ), #10679, .F. ) ;
#2845 = VERTEX_POINT ( 'NONE', #15204 ) ;
#2846 = CARTESIAN_POINT ( 'NONE',  ( -13.35725562635142794, -21.48433729119796709, -0.5488224920830401254 ) ) ;
#2847 = DIRECTION ( 'NONE',  ( -1.000000000000000000, 0.000000000000000000, 0.000000000000000000 ) ) ;
#2848 = ORIENTED_EDGE ( 'NONE', *, *, #957, .F. ) ;
#2849 = CARTESIAN_POINT ( 'NONE',  ( -13.75000000000000000, -35.50000000000000000, 5.500000000000000000 ) ) ;
#2850 = PRODUCT ( 'Spring-Loaded Carriage Elevator Arm', 'Spring-Loaded Carriage Elevator Arm', '', ( #2952 ) ) ;
#2851 = ORIENTED_EDGE ( 'NONE', *, *, #4080, .T. ) ;
#2852 = DIRECTION ( 'NONE',  ( -0.000000000000000000, 1.000000000000000000, -0.000000000000000000 ) ) ;
#2853 = DIRECTION ( 'NONE',  ( -0.000000000000000000, -0.000000000000000000, -1.000000000000000000 ) ) ;
#2854 = FACE_OUTER_BOUND ( 'NONE', #12466, .T. ) ;
#2855 = VECTOR ( 'NONE', #311, 1000.000000000000000 ) ;
#2856 = SHAPE_DEFINITION_REPRESENTATION ( #9125, #7912 ) ;
#2857 = DIRECTION ( 'NONE',  ( -1.156482317317871478E-16, 1.000000000000000000, 0.000000000000000000 ) ) ;
#2858 = CARTESIAN_POINT ( 'NONE',  ( -10.75228648362910100, -26.64274437364854009, 27.01367750791695954 ) ) ;
#2859 = DIRECTION ( 'NONE',  ( 0.000000000000000000, -0.000000000000000000, 1.000000000000000000 ) ) ;
#2860 = EDGE_CURVE ( 'NONE', #5958, #717, #4624, .T. ) ;
#2861 = CARTESIAN_POINT ( 'NONE',  ( -16.17491895705301275, -18.95583473709189803, 9.294927507916954212 ) ) ;
#2862 = CARTESIAN_POINT ( 'NONE',  ( -15.00000000000000000, 49.99999999999997158, -4.956352788505161414E-14 ) ) ;
#2863 = ORIENTED_EDGE ( 'NONE', *, *, #8533, .T. ) ;
#2864 = CARTESIAN_POINT ( 'NONE',  ( -19.41254052147350961, -21.64274437364857562, 5.361322492083041347 ) ) ;
#2865 = VECTOR ( 'NONE', #1641, 1000.000000000000000 ) ;
#2866 = CARTESIAN_POINT ( 'NONE',  ( -20.04416526290808065, -25.17491895705300209, 39.48242750791695244 ) ) ;
#2867 = CARTESIAN_POINT ( 'NONE',  ( 2.066987300000001859, 64.85617417291294373, 46.00000000109246656 ) ) ;
#2868 = CARTESIAN_POINT ( 'NONE',  ( -17.99999999999999645, -24.16482700510260173, 4.923822492083043123 ) ) ;
#2869 = VECTOR ( 'NONE', #8507, 1000.000000000000000 ) ;
#2870 = CARTESIAN_POINT ( 'NONE',  ( 4.999999999999999112, 0.000000000000000000, 0.000000000000000000 ) ) ;
#2871 = EDGE_LOOP ( 'NONE', ( #6456, #5564, #15323, #12070 ) ) ;
#2872 = CARTESIAN_POINT ( 'NONE',  ( -11.89515593330241749, -18.98492275559260989, 1.100789300500590883E-12 ) ) ;
#2873 = ORIENTED_EDGE ( 'NONE', *, *, #14905, .T. ) ;
#2874 = CARTESIAN_POINT ( 'NONE',  ( -11.46040770435012668, -27.78091578003887463, 37.73242750791694533 ) ) ;
#2875 = CARTESIAN_POINT ( 'NONE',  ( 37.50000000000000711, -6.000000000000000000, -47.50000000000000000 ) ) ;
#2876 = LINE ( 'NONE', #2581, #2 ) ;
#2877 = CARTESIAN_POINT ( 'NONE',  ( -41.00000000000000711, 110.0000000000000000, 20.00000000000000000 ) ) ;
#2878 = CARTESIAN_POINT ( 'NONE',  ( -11.21908421996106142, -27.53959229564982181, 39.70507249208304046 ) ) ;
#2879 = CARTESIAN_POINT ( 'NONE',  ( -2.500000000000001776, 65.03553390593273775, 47.54999999999999716 ) ) ;
#2880 = CARTESIAN_POINT ( 'NONE',  ( -0.8561741729129461742, 66.06698730000000808, 45.60000000109246798 ) ) ;
#2881 = FACE_BOUND ( 'NONE', #9818, .T. ) ;
#2882 = CARTESIAN_POINT ( 'NONE',  ( -1.767766952966370209, 65.76776695296638309, 47.49999999999999289 ) ) ;
#2883 = DIRECTION ( 'NONE',  ( -2.775557561562890858E-16, 0.7071067811865454633, 0.7071067811865496822 ) ) ;
#2884 = VECTOR ( 'NONE', #10918, 1000.000000000000000 ) ;
#2885 = ORIENTED_EDGE ( 'NONE', *, *, #11765, .F. ) ;
#2886 = EDGE_CURVE ( 'NONE', #13949, #5657, #9117, .T. ) ;
#2887 = ADVANCED_FACE ( 'NONE', ( #10384 ), #11750, .T. ) ;
#2888 = PRESENTATION_STYLE_ASSIGNMENT (( #10032 ) ) ;
#2889 = CARTESIAN_POINT ( 'NONE',  ( -13.49542703274178379, -19.04416526290806289, -0.7675724920830416798 ) ) ;
#2890 = AXIS2_PLACEMENT_3D ( 'NONE', #12031, #18028, #10559 ) ;
#2891 = CARTESIAN_POINT ( 'NONE',  ( -19.99999999999999645, -23.83517299489738051, 18.70117750791695954 ) ) ;
#2892 = CARTESIAN_POINT ( 'NONE',  ( -1.530808498934192803E-16, 66.50000000000000000, 47.50000000218494023 ) ) ;
#2893 = EDGE_CURVE ( 'NONE', #18722, #72, #1482, .T. ) ;
#2894 = CARTESIAN_POINT ( 'NONE',  ( -11.21908421996106320, -27.53959229564982181, 8.205072492083036906 ) ) ;
#2895 = CARTESIAN_POINT ( 'NONE',  ( 0.1249999999999895917, 33.84290755733280065, 52.64142146683631296 ) ) ;
#2896 = CARTESIAN_POINT ( 'NONE',  ( -19.95583473709191580, -22.49542703274176603, 8.419927507916955989 ) ) ;
#2897 = CARTESIAN_POINT ( 'NONE',  ( -12.35725562635143682, -19.75228648362908501, 4.701177507916957765 ) ) ;
#2898 = LINE ( 'NONE', #19369, #6240 ) ;
#2899 = DIRECTION ( 'NONE',  ( -0.000000000000000000, 0.7071067811865456854, 0.7071067811865493491 ) ) ;
#2900 = CARTESIAN_POINT ( 'NONE',  ( -40.00000000000000000, 53.00000000000000711, 30.00000000000000000 ) ) ;
#2901 = DIRECTION ( 'NONE',  ( -0.000000000000000000, -1.000000000000000000, -0.000000000000000000 ) ) ;
#2902 = ADVANCED_FACE ( 'NONE', ( #10578 ), #1676, .T. ) ;
#2903 = CARTESIAN_POINT ( 'NONE',  ( 7.500000000000005329, -26.00000000000000000, 12.50000000000000000 ) ) ;
#2904 = CARTESIAN_POINT ( 'NONE',  ( -0.8561741729129461742, 66.06698729999999387, 49.60000000109246798 ) ) ;
#2905 = EDGE_CURVE ( 'NONE', #13286, #2004, #9310, .T. ) ;
#2906 = PLANE ( 'NONE',  #10182 ) ;
#2907 = ORIENTED_EDGE ( 'NONE', *, *, #12486, .F. ) ;
#2908 = VERTEX_POINT ( 'NONE', #9689 ) ;
#2909 = CARTESIAN_POINT ( 'NONE',  ( -8.855408670957602979, -27.35725562635137820, 23.73632249208303691 ) ) ;
#2910 = LINE ( 'NONE', #5956, #15679 ) ;
#2912 = ORIENTED_EDGE ( 'NONE', *, *, #12038, .T. ) ;
#2911 = VERTEX_POINT ( 'NONE', #2059 ) ;
#2913 = EDGE_CURVE ( 'NONE', #16200, #15859, #6576, .T. ) ;
#2914 = CARTESIAN_POINT ( 'NONE',  ( -11.95583473709191047, -23.36097942780921954, 21.10742750791696309 ) ) ;
#2915 = CARTESIAN_POINT ( 'NONE',  ( -10.00000000000000000, 0.000000000000000000, 0.000000000000000000 ) ) ;
#2916 = CARTESIAN_POINT ( 'NONE',  ( -20.00369391078757886, -29.24501739517668142, 9.517572492083038682 ) ) ;
#2917 = DIRECTION ( 'NONE',  ( -0.000000000000000000, -1.000000000000000000, -0.000000000000000000 ) ) ;
#2918 = CARTESIAN_POINT ( 'NONE',  ( -1.265664690411616068E-16, 66.06698730000000808, 48.55000000109247082 ) ) ;
#2919 = ORIENTED_EDGE ( 'NONE', *, *, #1250, .F. ) ;
#2920 = ORIENTED_EDGE ( 'NONE', *, *, #11885, .T. ) ;
#2921 = CARTESIAN_POINT ( 'NONE',  ( 2.500000000000001776, 64.00000000000000000, 47.19999999999999574 ) ) ;
#2922 = CARTESIAN_POINT ( 'NONE',  ( -41.00000000000000000, 47.00000000000000711, -67.72004514666936359 ) ) ;
#2923 = ORIENTED_EDGE ( 'NONE', *, *, #26, .F. ) ;
#2924 = CARTESIAN_POINT ( 'NONE',  ( -14.11162457711532703, -20.06223238837476330, 1.106825084037506213E-14 ) ) ;
#2925 = CARTESIAN_POINT ( 'NONE',  ( -40.00000000000000000, 53.00000000000000711, 0.5000000000000004441 ) ) ;
#2926 = CARTESIAN_POINT ( 'NONE',  ( -0.8561741729129461742, 66.06698729999999387, 48.80000000109247082 ) ) ;
#2927 = EDGE_CURVE ( 'NONE', #3230, #15072, #9595, .T. ) ;
#2928 = EDGE_CURVE ( 'NONE', #12056, #2690, #12635, .T. ) ;
#2929 = CARTESIAN_POINT ( 'NONE',  ( 0.08838834764830766355, 29.80514068711926257, 56.68014068711929809 ) ) ;
#2930 = CARTESIAN_POINT ( 'NONE',  ( -1.040834085586084257E-14, 33.84386001800124433, 51.22720779386423118 ) ) ;
#2931 = VERTEX_POINT ( 'NONE', #7854 ) ;
#2933 = VERTEX_POINT ( 'NONE', #3431 ) ;
#2932 = ORIENTED_EDGE ( 'NONE', *, *, #19177, .F. ) ;
#2934 = EDGE_CURVE ( 'NONE', #13522, #8266, #17844, .T. ) ;
#2935 = CARTESIAN_POINT ( 'NONE',  ( -8.044165262908075320, -26.04047135212042718, 21.54492750791695599 ) ) ;
#2936 = FACE_OUTER_BOUND ( 'NONE', #12656, .T. ) ;
#2937 = ORIENTED_EDGE ( 'NONE', *, *, #659, .F. ) ;
#2938 = VERTEX_POINT ( 'NONE', #11156 ) ;
#2939 = CARTESIAN_POINT ( 'NONE',  ( -12.92450931948790149, -21.68318583509881137, 22.64257249208304401 ) ) ;
#2940 = DIRECTION ( 'NONE',  ( 0.000000000000000000, -0.5000000000000013323, -0.8660254037844378194 ) ) ;
#2941 = DIRECTION ( 'NONE',  ( 0.000000000000000000, 0.000000000000000000, 1.000000000000000000 ) ) ;
#2942 = ORIENTED_EDGE ( 'NONE', *, *, #5989, .T. ) ;
#2943 = CARTESIAN_POINT ( 'NONE',  ( -16.64274437364856496, -26.51566270880199738, 7.326177507916959541 ) ) ;
#2944 = CARTESIAN_POINT ( 'NONE',  ( -40.00000000000000711, 113.0000000000000000, -45.00000000000000000 ) ) ;
#2945 = EDGE_LOOP ( 'NONE', ( #9798, #14980, #7780, #17743, #13882 ) ) ;
#2946 = FACE_OUTER_BOUND ( 'NONE', #11157, .T. ) ;
#2947 = ORIENTED_EDGE ( 'NONE', *, *, #7881, .T. ) ;
#2948 = EDGE_CURVE ( 'NONE', #15781, #8882, #6477, .T. ) ;
#2949 = LINE ( 'NONE', #11665, #3785 ) ;
#2950 = PLANE ( 'NONE',  #16446 ) ;
#2951 = DIRECTION ( 'NONE',  ( -0.000000000000000000, -0.000000000000000000, -1.000000000000000000 ) ) ;
#2952 = PRODUCT_CONTEXT ( 'NONE', #10703, 'mechanical' ) ;
#2953 = CARTESIAN_POINT ( 'NONE',  ( -1.035533905932738863, 61.50000000000000000, 46.25000000218494733 ) ) ;
#2954 = DIRECTION ( 'NONE',  ( -0.000000000000000000, -0.000000000000000000, -1.000000000000000000 ) ) ;
#2955 = MECHANICAL_DESIGN_GEOMETRIC_PRESENTATION_REPRESENTATION (  '', ( #14850 ), #2008 ) ;
#2956 = CARTESIAN_POINT ( 'NONE',  ( -41.00000000000000711, 53.00000000000000711, 14.50000000000000000 ) ) ;
#2957 = CARTESIAN_POINT ( 'NONE',  ( -19.99999999999999645, -23.83517299489738051, 18.70117750791695954 ) ) ;
#2958 = DIRECTION ( 'NONE',  ( -0.000000000000000000, -0.000000000000000000, -1.000000000000000000 ) ) ;
#2959 = ORIENTED_EDGE ( 'NONE', *, *, #11929, .F. ) ;
#2960 = CARTESIAN_POINT ( 'NONE',  ( -13.49542703274174116, -28.95583473709188738, 3.392572492083040903 ) ) ;
#2961 = CARTESIAN_POINT ( 'NONE',  ( -2.066987300000001415, 64.00000000000000000, 46.35000000109246798 ) ) ;
#2962 = CARTESIAN_POINT ( 'NONE',  ( -13.49542703274174116, -28.95583473709188738, 40.14257249208304756 ) ) ;
#2963 = CARTESIAN_POINT ( 'NONE',  ( -1.530808498934192803E-16, 66.50000000000000000, 45.79999999999999005 ) ) ;
#2964 = EDGE_LOOP ( 'NONE', ( #14334, #15183, #19116, #15483 ) ) ;
#2965 = CIRCLE ( 'NONE', #7668, 1.500000000000001332 ) ;
#2966 = DIRECTION ( 'NONE',  ( 0.000000000000000000, 1.000000000000000000, -0.000000000000000000 ) ) ;
#2967 = ORIENTED_EDGE ( 'NONE', *, *, #57, .T. ) ;
#2968 = CARTESIAN_POINT ( 'NONE',  ( -10.00000000000000000, 50.00000000000000711, 37.00000000000000000 ) ) ;
#2969 = CARTESIAN_POINT ( 'NONE',  ( 14.99999999999998579, 73.00000000000001421, 20.99999999999997513 ) ) ;
#2970 = CARTESIAN_POINT ( 'NONE',  ( -1.035533905932738863, 61.50000000000000000, 45.34999999999998721 ) ) ;
#2971 =( BOUNDED_CURVE ( )  B_SPLINE_CURVE ( 2, ( #11661, #5892, #10282, #16179, #16381 ),
 .UNSPECIFIED., .F., .F. ) 
 B_SPLINE_CURVE_WITH_KNOTS ( ( 3, 2, 3 ),
 ( 0.8571428571428568732, 0.8749999999999998890, 0.8928571428571429047 ),
 .UNSPECIFIED. ) 
 CURVE ( )  GEOMETRIC_REPRESENTATION_ITEM ( )  RATIONAL_B_SPLINE_CURVE ( ( 1.000000000000000888, 0.9238795325112857393, 1.000000000000000000, 0.9238795325112867385, 1.000000000000000000 ) ) 
 REPRESENTATION_ITEM ( '' )  );
#2972 = DIRECTION ( 'NONE',  ( 0.000000000000000000, -1.000000000000000000, 0.000000000000000000 ) ) ;
#2973 = FACE_OUTER_BOUND ( 'NONE', #9281, .T. ) ;
#2974 = CARTESIAN_POINT ( 'NONE',  ( -2.066987300000000971, 63.14382582708704916, 47.40000000109247225 ) ) ;
#2975 = SURFACE_STYLE_USAGE ( .BOTH. , #1416 ) ;
#2976 = CARTESIAN_POINT ( 'NONE',  ( 1.767766952966370653, 62.23223304703363112, 47.89999999999999858 ) ) ;
#2977 = CARTESIAN_POINT ( 'NONE',  ( 12.55500000000001748, 0.000000000000000000, 0.000000000000000000 ) ) ;
#2978 = PRODUCT_DEFINITION_FORMATION_WITH_SPECIFIED_SOURCE ( 'ANY', '', #2850, .NOT_KNOWN. ) ;
#2979 = VECTOR ( 'NONE', #6699, 999.9999999999997726 ) ;
#2980 = VERTEX_POINT ( 'NONE', #3716 ) ;
#2981 = CARTESIAN_POINT ( 'NONE',  ( -13.49542703274178379, -19.04416526290806289, 9.732427507916959541 ) ) ;
#2982 = CARTESIAN_POINT ( 'NONE',  ( -16.17491895705301275, -18.95583473709189803, 19.79492750791695954 ) ) ;
#2983 = CARTESIAN_POINT ( 'NONE',  ( -0.1886580908559672143, 66.48422237085870279, 45.00000000000000711 ) ) ;
#2984 = CARTESIAN_POINT ( 'NONE',  ( -12.64274437364858628, -19.58745947852646552, 6.673822492083040459 ) ) ;
#2985 = CARTESIAN_POINT ( 'NONE',  ( -2.066987300000001415, 63.14382582708705627, 46.60000000109246088 ) ) ;
#2986 = CARTESIAN_POINT ( 'NONE',  ( -18.78091578003889950, -27.53959229564985378, 2.294927507916958209 ) ) ;
#2987 = DIRECTION ( 'NONE',  ( -0.000000000000000000, -0.000000000000000000, -1.000000000000000000 ) ) ;
#2988 = AXIS2_PLACEMENT_3D ( 'NONE', #17735, #16463, #11739 ) ;
#2989 = CARTESIAN_POINT ( 'NONE',  ( -14.83517299489739649, -18.99999999999997868, 4.263677507916958653 ) ) ;
#2990 = DIRECTION ( 'NONE',  ( 8.163404592832032733E-17, -0.000000000000000000, 1.000000000000000000 ) ) ;
#2991 = VECTOR ( 'NONE', #11645, 1000.000000000000000 ) ;
#2992 = DIRECTION ( 'NONE',  ( -0.000000000000000000, -0.000000000000000000, -1.000000000000000000 ) ) ;
#2993 = CARTESIAN_POINT ( 'NONE',  ( -25.00000000000000711, 110.0000000000000000, 6.999999999999999112 ) ) ;
#2994 = EDGE_CURVE ( 'NONE', #12352, #18999, #18441, .T. ) ;
#2995 = DIRECTION ( 'NONE',  ( 0.8660254037844385966, 0.000000000000000000, 0.5000000000000001110 ) ) ;
#2996 = CARTESIAN_POINT ( 'NONE',  ( 2.066987300000001415, 64.00000000000000000, 45.35000000109246798 ) ) ;
#2997 = CARTESIAN_POINT ( 'NONE',  ( -3.155775640247338920, -38.39960408384397539, 3.000000000000000000 ) ) ;
#2998 = ADVANCED_FACE ( 'NONE', ( #400 ), #14012, .F. ) ;
#2999 = CARTESIAN_POINT ( 'NONE',  ( 1.767766952966370653, 62.23223304703363112, 44.80000000218493739 ) ) ;
#3000 = ORIENTED_EDGE ( 'NONE', *, *, #2473, .F. ) ;
#3001 = VERTEX_POINT ( 'NONE', #18344 ) ;
#3002 = CARTESIAN_POINT ( 'NONE',  ( -21.14459132904239169, -20.64274437364858628, 15.86132249208304223 ) ) ;
#3003 = EDGE_CURVE ( 'NONE', #17432, #18408, #4914, .T. ) ;
#3004 = VECTOR ( 'NONE', #4487, 1000.000000000000000 ) ;
#3005 = VECTOR ( 'NONE', #8364, 1000.000000000000000 ) ;
#3006 = CARTESIAN_POINT ( 'NONE',  ( -9.999999999999994671, -23.83517299489734143, 2.298822492083040903 ) ) ;
#3008 = VERTEX_POINT ( 'NONE', #18544 ) ;
#3007 = VERTEX_POINT ( 'NONE', #15398 ) ;
#3009 = PRODUCT_DEFINITION_SHAPE ( 'NONE', 'NONE',  #19403 ) ;
#3010 = CARTESIAN_POINT ( 'NONE',  ( -17.99999999999999645, -23.83517299489736985, 18.70117750791695599 ) ) ;
#3011 = CARTESIAN_POINT ( 'NONE',  ( -1.767766952966369765, 62.23223304703363112, 48.60000000218494165 ) ) ;
#3012 = CARTESIAN_POINT ( 'NONE',  ( -18.64274437364853654, -29.97976432393976509, 38.82617750791695244 ) ) ;
#3013 = B_SPLINE_CURVE_WITH_KNOTS ( 'NONE', 3,
 ( #11207, #2485, #17481, #8287 ),
 .UNSPECIFIED., .F., .F.,
 ( 4, 4 ),
 ( 0.000000000000000000, 1.000000000000000000 ),
 .UNSPECIFIED. ) ;
#3014 = CARTESIAN_POINT ( 'NONE',  ( -2.066987300000001859, 64.85617417291294373, 49.50000000109246656 ) ) ;
#3015 = CARTESIAN_POINT ( 'NONE',  ( -1.767766952966370209, 65.76776695296638309, 44.40000000218493881 ) ) ;
#3016 = ORIENTED_EDGE ( 'NONE', *, *, #9343, .F. ) ;
#3017 = VERTEX_POINT ( 'NONE', #5009 ) ;
#3018 = LINE ( 'NONE', #13299, #18825 ) ;
#3019 = FACE_OUTER_BOUND ( 'NONE', #17852, .T. ) ;
#3020 = ORIENTED_EDGE ( 'NONE', *, *, #8179, .F. ) ;
#3021 = CARTESIAN_POINT ( 'NONE',  ( -32.50000000000001421, 0.000000000000000000, 44.99999999999997868 ) ) ;
#3022 = DIRECTION ( 'NONE',  ( 0.000000000000000000, 1.000000000000000000, 0.000000000000000000 ) ) ;
#3023 = ADVANCED_FACE ( 'NONE', ( #12254 ), #10968, .T. ) ;
#3024 = VECTOR ( 'NONE', #18924, 1000.000000000000000 ) ;
#3025 = CARTESIAN_POINT ( 'NONE',  ( 2.066987300000001415, 64.00000000000000000, 47.75000000109246656 ) ) ;
#3026 = CIRCLE ( 'NONE', #13984, 2.999999999999999112 ) ;
#3027 = CARTESIAN_POINT ( 'NONE',  ( -40.00000000000000711, 110.0000000000000000, 30.00000000000000000 ) ) ;
#3028 = CARTESIAN_POINT ( 'NONE',  ( -43.50000000000000000, 115.0000000000000000, 32.50000000000000000 ) ) ;
#3029 = ORIENTED_EDGE ( 'NONE', *, *, #17851, .T. ) ;
#3031 = ORIENTED_EDGE ( 'NONE', *, *, #12037, .T. ) ;
#3030 = ORIENTED_EDGE ( 'NONE', *, *, #15550, .T. ) ;
#3032 = CARTESIAN_POINT ( 'NONE',  ( -9.996306089212364299, -29.24501739517662813, 11.48242750791695777 ) ) ;
#3033 = DIRECTION ( 'NONE',  ( 0.000000000000000000, 0.000000000000000000, -1.000000000000000000 ) ) ;
#3034 = ORIENTED_EDGE ( 'NONE', *, *, #1039, .F. ) ;
#3035 = VERTEX_POINT ( 'NONE', #14114 ) ;
#3036 = CARTESIAN_POINT ( 'NONE',  ( -14.36097942780925685, -20.95583473709189093, 11.70507249208304223 ) ) ;
#3037 = PRESENTATION_LAYER_ASSIGNMENT (  '', '', ( #6795 ) ) ;
#3038 = ADVANCED_FACE ( 'NONE', ( #18250 ), #12543, .F. ) ;
#3039 = ADVANCED_FACE ( 'NONE', ( #9501 ), #11064, .T. ) ;
#3040 = DIRECTION ( 'NONE',  ( 0.000000000000000000, -0.7071067811865455743, -0.7071067811865495711 ) ) ;
#3041 = FACE_OUTER_BOUND ( 'NONE', #4414, .T. ) ;
#3042 = EDGE_LOOP ( 'NONE', ( #2907, #7887, #6384, #15431 ) ) ;
#3043 = ADVANCED_FACE ( 'NONE', ( #14207 ), #10769, .T. ) ;
#3044 = CARTESIAN_POINT ( 'NONE',  ( -17.95583473709191580, -23.03132541760400898, 18.91992750791695954 ) ) ;
#3045 = LINE ( 'NONE', #9019, #4094 ) ;
#3046 = ORIENTED_EDGE ( 'NONE', *, *, #10797, .T. ) ;
#3047 = FACE_OUTER_BOUND ( 'NONE', #13827, .T. ) ;
#3048 = ORIENTED_EDGE ( 'NONE', *, *, #16453, .F. ) ;
#3049 = CARTESIAN_POINT ( 'NONE',  ( 8.000000000000000000, 68.00000000000000000, 45.00000000000000000 ) ) ;
#3050 = DIRECTION ( 'NONE',  ( -1.000000000000000000, 0.000000000000000000, 0.000000000000000000 ) ) ;
#3051 = DIRECTION ( 'NONE',  ( 1.156482317317871725E-16, 0.000000000000000000, -1.000000000000000000 ) ) ;
#3052 = PRODUCT_CONTEXT ( 'NONE', #7058, 'mechanical' ) ;
#3053 = DIRECTION ( 'NONE',  ( -1.156482317317871478E-16, 1.000000000000000000, 0.000000000000000000 ) ) ;
#3054 = CARTESIAN_POINT ( 'NONE',  ( -1.767766952966370209, 65.76776695296638309, 48.29999999999999716 ) ) ;
#3055 = DIRECTION ( 'NONE',  ( 0.000000000000000000, -1.000000000000000000, 0.000000000000000000 ) ) ;
#3056 = CARTESIAN_POINT ( 'NONE',  ( -18.78091578003889950, -27.53959229564985378, 23.29492750791695954 ) ) ;
#3057 = CARTESIAN_POINT ( 'NONE',  ( -43.50000000000000711, 115.0000000000000000, -52.50000000000000711 ) ) ;
#3058 = VERTEX_POINT ( 'NONE', #16771 ) ;
#3059 = EDGE_CURVE ( 'NONE', #7257, #17715, #2526, .T. ) ;
#3060 = CARTESIAN_POINT ( 'NONE',  ( -11.21908421996106320, -27.53959229564982181, 23.95507249208304401 ) ) ;
#3061 =( REPRESENTATION_RELATIONSHIP ('NONE','NONE', #7912, #6533 ) REPRESENTATION_RELATIONSHIP_WITH_TRANSFORMATION ( #18452 )SHAPE_REPRESENTATION_RELATIONSHIP( ) );
#3062 = EDGE_CURVE ( 'NONE', #3881, #13516, #17247, .T. ) ;
#3063 = CARTESIAN_POINT ( 'NONE',  ( 0.04165538583019261221, 25.64078660347668759, 60.84386001800125854 ) ) ;
#3064 = CARTESIAN_POINT ( 'NONE',  ( -16.64274437364858272, -21.48433729119797420, 11.04882249208304223 ) ) ;
#3065 = CARTESIAN_POINT ( 'NONE',  ( 44.99999999999998579, 6.000000000000000000, -54.99999999999998579 ) ) ;
#3066 = VERTEX_POINT ( 'NONE', #15868 ) ;
#3067 = CARTESIAN_POINT ( 'NONE',  ( -14.39797529960427269, -18.02527416137649396, 9.743381756881009494E-15 ) ) ;
#3068 = ORIENTED_EDGE ( 'NONE', *, *, #11028, .F. ) ;
#3069 = CARTESIAN_POINT ( 'NONE',  ( 50.00000000000000000, 118.0000000000000142, -60.00000000000000000 ) ) ;
#3070 = CARTESIAN_POINT ( 'NONE',  ( -41.00000000000000711, 53.00000000000000711, -30.99999999999999645 ) ) ;
#3071 = CARTESIAN_POINT ( 'NONE',  ( -25.00000000000000000, 113.0000000000000000, -50.00000000000000000 ) ) ;
#3072 = DIRECTION ( 'NONE',  ( 0.000000000000000000, 1.000000000000000000, -1.224646799147353207E-16 ) ) ;
#3073 = CARTESIAN_POINT ( 'NONE',  ( -1.265664690411616068E-16, 66.06698730000000808, 45.55000000109246372 ) ) ;
#3074 = DIRECTION ( 'NONE',  ( -0.000000000000000000, -0.000000000000000000, -1.000000000000000000 ) ) ;
#3075 = CARTESIAN_POINT ( 'NONE',  ( 2.500000000000001776, 64.00000000000000000, 47.99999999999999289 ) ) ;
#3076 = CARTESIAN_POINT ( 'NONE',  ( -2.500000000000001776, 64.00000000000000000, 49.99999999999999289 ) ) ;
#3077 = ADVANCED_FACE ( 'NONE', ( #5388 ), #19099, .F. ) ;
#3078 = ORIENTED_EDGE ( 'NONE', *, *, #15657, .F. ) ;
#3079 = VECTOR ( 'NONE', #8379, 1000.000000000000000 ) ;
#3080 = CARTESIAN_POINT ( 'NONE',  ( -17.35725562635144215, -19.58745947852648683, 3.826177507916958209 ) ) ;
#3081 = CARTESIAN_POINT ( 'NONE',  ( -16.50457296725820555, -28.95583473709189448, 12.35742750791695954 ) ) ;
#3082 = CARTESIAN_POINT ( 'NONE',  ( 1.035533905932739751, 61.50000000000000000, 47.95000000218495018 ) ) ;
#3083 = CARTESIAN_POINT ( 'NONE',  ( -21.99999999999999289, -24.16482700510262305, 41.67382249208304756 ) ) ;
#3084 = CARTESIAN_POINT ( 'NONE',  ( -0.8561741729129461742, 66.06698729999999387, 46.40000000109246514 ) ) ;
#3085 = CARTESIAN_POINT ( 'NONE',  ( -20.04416526290808065, -25.17491895705300209, 7.982427507916958653 ) ) ;
#3086 = CARTESIAN_POINT ( 'NONE',  ( -2.315774708385926139, 31.50514068711928672, 54.98014068711927393 ) ) ;
#3088 = AXIS2_PLACEMENT_3D ( 'NONE', #17603, #19073, #19273 ) ;
#3087 = CARTESIAN_POINT ( 'NONE',  ( -9.999999999999994671, -24.16482700510257686, 21.32617750791695599 ) ) ;
#3089 = LINE ( 'NONE', #17907, #18761 ) ;
#3090 = CARTESIAN_POINT ( 'NONE',  ( -17.70357423236093553, -43.78611686177728046, 3.000000000000000000 ) ) ;
#3091 = CARTESIAN_POINT ( 'NONE',  ( 0.1249999999999895917, 32.14680374315353362, 54.33847763108504125 ) ) ;
#3092 = AXIS2_PLACEMENT_3D ( 'NONE', #7588, #13453, #10114 ) ;
#3093 = DIRECTION ( 'NONE',  ( 0.000000000000000000, -0.000000000000000000, -1.000000000000000000 ) ) ;
#3094 = CARTESIAN_POINT ( 'NONE',  ( -1.461580736456473462, 62.53841926354353120, 46.65000000109247225 ) ) ;
#3095 = CARTESIAN_POINT ( 'NONE',  ( -19.99999999999999645, -52.00000000000000711, 1.500000000000000000 ) ) ;
#3096 = LINE ( 'NONE', #927, #18665 ) ;
#3097 = EDGE_CURVE ( 'NONE', #6553, #9106, #773, .T. ) ;
#3098 = CARTESIAN_POINT ( 'NONE',  ( -40.00000000000000711, 110.0000000000000000, 14.50000000000000000 ) ) ;
#3100 = VERTEX_POINT ( 'NONE', #9874 ) ;
#3099 = EDGE_CURVE ( 'NONE', #9583, #9953, #9783, .T. ) ;
#3101 = EDGE_LOOP ( 'NONE', ( #19144, #17751, #13426, #18140 ) ) ;
#3102 = CARTESIAN_POINT ( 'NONE',  ( -16.71081734191520596, -31.04416526290808065, 19.58007249208303691 ) ) ;
#3103 = VECTOR ( 'NONE', #8262, 1000.000000000000000 ) ;
#3104 = SHAPE_REPRESENTATION_RELATIONSHIP ( 'NONE' , 'NONE' ,  #9996, #4072 ) ;
#3105 = CARTESIAN_POINT ( 'NONE',  ( -10.58745947852648328, -26.35725562635138530, 2.736322492083041347 ) ) ;
#3107 = ORIENTED_EDGE ( 'NONE', *, *, #16225, .T. ) ;
#3106 = EDGE_LOOP ( 'NONE', ( #14869, #7316, #14335, #3048 ) ) ;
#3108 = CARTESIAN_POINT ( 'NONE',  ( -14.03132541760401786, -21.04416526290806289, 14.98242750791695954 ) ) ;
#3109 = CARTESIAN_POINT ( 'NONE',  ( 2.500000000000001776, 64.00000000000000000, 48.90000000218494591 ) ) ;
#3110 = CARTESIAN_POINT ( 'NONE',  ( -11.64274437364859693, -17.85540867095757989, 6.673822492083038682 ) ) ;
#3111 = AXIS2_PLACEMENT_3D ( 'NONE', #14326, #14514, #894 ) ;
#3112 = VECTOR ( 'NONE', #11226, 1000.000000000000000 ) ;
#3113 = CARTESIAN_POINT ( 'NONE',  ( 3.796994071234847710E-16, 61.93301269999999903, 48.15000000109247225 ) ) ;
#3114 = CARTESIAN_POINT ( 'NONE',  ( 2.066987300000001415, 64.00000000000000000, 46.75000000109247367 ) ) ;
#3115 = VERTEX_POINT ( 'NONE', #4102 ) ;
#3116 = ORIENTED_EDGE ( 'NONE', *, *, #7505, .T. ) ;
#3117 = LINE ( 'NONE', #7330, #977 ) ;
#3118 = DIRECTION ( 'NONE',  ( -1.000000000000000000, 0.000000000000000000, 0.000000000000000000 ) ) ;
#3119 = ORIENTED_EDGE ( 'NONE', *, *, #4240, .F. ) ;
#3120 = CARTESIAN_POINT ( 'NONE',  ( -13.46816481875853277, -20.24306461418997216, 1.106825084037506055E-14 ) ) ;
#3121 = DIRECTION ( 'NONE',  ( 0.000000000000000000, -0.000000000000000000, -1.000000000000000000 ) ) ;
#3122 = VECTOR ( 'NONE', #8349, 1000.000000000000000 ) ;
#3123 = CARTESIAN_POINT ( 'NONE',  ( 0.8561741729129460632, 66.06698729999999387, 46.30000000109247082 ) ) ;
#3124 = DIRECTION ( 'NONE',  ( 0.000000000000000000, -0.7071067811865455743, -0.7071067811865495711 ) ) ;
#3125 = VECTOR ( 'NONE', #14120, 1000.000000000000000 ) ;
#3126 = CARTESIAN_POINT ( 'NONE',  ( -2.500000000000001776, 64.00000000000000000, 47.70000000218494307 ) ) ;
#3127 = EDGE_LOOP ( 'NONE', ( #7341, #13695, #17840, #4878 ) ) ;
#3129 = ORIENTED_EDGE ( 'NONE', *, *, #15264, .F. ) ;
#3128 = ORIENTED_EDGE ( 'NONE', *, *, #8748, .F. ) ;
#3130 = CARTESIAN_POINT ( 'NONE',  ( -9.754982604823348780, -18.99630608921234654, 10.16992750791695777 ) ) ;
#3131 = CARTESIAN_POINT ( 'NONE',  ( -0.1250000000000104083, 33.66708332270461312, 52.46464466094069934 ) ) ;
#3132 = VERTEX_POINT ( 'NONE', #18721 ) ;
#3133 = VECTOR ( 'NONE', #11633, 1000.000000000000000 ) ;
#3134 = ORIENTED_EDGE ( 'NONE', *, *, #15716, .T. ) ;
#3135 = CARTESIAN_POINT ( 'NONE',  ( -16.64274437364858272, -21.48433729119797420, 16.29882249208304401 ) ) ;
#3136 = EDGE_CURVE ( 'NONE', #6673, #15600, #5474, .T. ) ;
#3137 = ADVANCED_FACE ( 'NONE', ( #7132 ), #2342, .T. ) ;
#3138 = LINE ( 'NONE', #14011, #12507 ) ;
#3139 = CARTESIAN_POINT ( 'NONE',  ( -41.00000000000000711, 53.00000000000000711, -12.50000000000000000 ) ) ;
#3140 = ORIENTED_EDGE ( 'NONE', *, *, #11983, .F. ) ;
#3141 = CARTESIAN_POINT ( 'NONE',  ( -17.68048971390461688, -25.35725562635141372, 23.51367750791696309 ) ) ;
#3142 = AXIS2_PLACEMENT_3D ( 'NONE', #15308, #11169, #5024 ) ;
#3143 = DIRECTION ( 'NONE',  ( -1.000000000000000000, 0.000000000000000000, -2.081668171172167774E-16 ) ) ;
#3144 = ORIENTED_EDGE ( 'NONE', *, *, #7068, .T. ) ;
#3145 = DIRECTION ( 'NONE',  ( -0.000000000000000000, -1.000000000000000000, -0.000000000000000000 ) ) ;
#3146 = ORIENTED_EDGE ( 'NONE', *, *, #9778, .T. ) ;
#3147 = DIRECTION ( 'NONE',  ( 0.000000000000000000, 0.000000000000000000, 1.000000000000000000 ) ) ;
#3148 = DIRECTION ( 'NONE',  ( 0.000000000000000000, 0.000000000000000000, -1.000000000000000000 ) ) ;
#3149 = CARTESIAN_POINT ( 'NONE',  ( -2.500000000000001776, 64.00000000000000000, 49.99999999999999289 ) ) ;
#3150 = AXIS2_PLACEMENT_3D ( 'NONE', #8537, #6969, #14324 ) ;
#3151 = LINE ( 'NONE', #9515, #8966 ) ;
#3152 = DIRECTION ( 'NONE',  ( 0.000000000000000000, -1.000000000000000000, 0.000000000000000000 ) ) ;
#3153 = CIRCLE ( 'NONE', #6896, 2.499999999999998668 ) ;
#3154 = CARTESIAN_POINT ( 'NONE',  ( -9.999999999999994671, -24.16482700510257686, 37.07617750791695954 ) ) ;
#3155 = EDGE_CURVE ( 'NONE', #19093, #13301, #11437, .T. ) ;
#3156 = LINE ( 'NONE', #4239, #13581 ) ;
#3157 = EDGE_CURVE ( 'NONE', #2911, #15600, #13100, .T. ) ;
#3158 = CARTESIAN_POINT ( 'NONE',  ( -10.75228648362910100, -26.64274437364854009, 16.51367750791695954 ) ) ;
#3159 = EDGE_CURVE ( 'NONE', #11531, #10686, #1888, .T. ) ;
#3160 = STYLED_ITEM ( 'NONE', ( #4954 ), #10129 ) ;
#3161 = DIRECTION ( 'NONE',  ( 0.000000000000000000, -1.000000000000000000, 0.000000000000000000 ) ) ;
#3162 = ORIENTED_EDGE ( 'NONE', *, *, #13703, .F. ) ;
#3163 = CARTESIAN_POINT ( 'NONE',  ( -10.04416526290808953, -22.49542703274172695, 17.83007249208303691 ) ) ;
#3164 = VECTOR ( 'NONE', #15871, 1000.000000000000000 ) ;
#3165 = CARTESIAN_POINT ( 'NONE',  ( 4.072081901468789233, 32.66337542264476923, 53.82127119883322308 ) ) ;
#3166 = CARTESIAN_POINT ( 'NONE',  ( -13.64274437364857739, -21.31951028609534760, 11.92382249208304401 ) ) ;
#3167 = DIRECTION ( 'NONE',  ( 0.000000000000000000, 0.000000000000000000, -1.000000000000000000 ) ) ;
#3168 = EDGE_LOOP ( 'NONE', ( #11221, #15374, #4325, #14700 ) ) ;
#3169 = AXIS2_PLACEMENT_3D ( 'NONE', #17657, #4232, #3849 ) ;
#3170 = CYLINDRICAL_SURFACE ( 'NONE', #6872, 2.500000000000001776 ) ;
#3171 = VERTEX_POINT ( 'NONE', #2722 ) ;
#3172 = CARTESIAN_POINT ( 'NONE',  ( 1.300000000000000044, 1.478016689125442484, -1.626303258728256651E-15 ) ) ;
#3173 = LINE ( 'NONE', #11785, #472 ) ;
#3174 = VECTOR ( 'NONE', #4385, 1000.000000000000000 ) ;
#3175 = CARTESIAN_POINT ( 'NONE',  ( -24.00000000000000711, 53.00000000000000711, -44.00000000000000000 ) ) ;
#3176 = CARTESIAN_POINT ( 'NONE',  ( -1.461580736456473906, 65.46158073645646880, 46.45000000109246940 ) ) ;
#3177 = VECTOR ( 'NONE', #18325, 1000.000000000000114 ) ;
#3178 = ADVANCED_FACE ( 'NONE', ( #15776 ), #17337, .T. ) ;
#3179 = CARTESIAN_POINT ( 'NONE',  ( -24.00000000000000000, 53.00000000000000711, -44.00000000000000000 ) ) ;
#3180 = DIRECTION ( 'NONE',  ( 1.000000000000000000, 0.000000000000000000, -0.000000000000000000 ) ) ;
#3181 = CARTESIAN_POINT ( 'NONE',  ( -14.99999999999999645, 52.00000000000000711, 23.99999999999997868 ) ) ;
#3182 = VECTOR ( 'NONE', #6048, 1000.000000000000000 ) ;
#3183 = ORIENTED_EDGE ( 'NONE', *, *, #5411, .F. ) ;
#3184 = EDGE_CURVE ( 'NONE', #10801, #17922, #3906, .T. ) ;
#3185 = AXIS2_PLACEMENT_3D ( 'NONE', #8363, #2465, #5510 ) ;
#3186 = DIRECTION ( 'NONE',  ( 6.123233995736766036E-17, -1.000000000000000000, 0.000000000000000000 ) ) ;
#3187 = CARTESIAN_POINT ( 'NONE',  ( -19.99999999999999645, -23.83517299489738051, 23.95117750791695954 ) ) ;
#3188 = CARTESIAN_POINT ( 'NONE',  ( -15.16482700510259640, -28.99999999999998224, 12.13867750791695777 ) ) ;
#3189 = CARTESIAN_POINT ( 'NONE',  ( -1.035533905932738863, 61.50000000000000000, 47.85000000218494165 ) ) ;
#3190 = CARTESIAN_POINT ( 'NONE',  ( -12.35725562635140307, -28.24771351637085459, 13.67382249208304223 ) ) ;
#3191 = CARTESIAN_POINT ( 'NONE',  ( -0.8561741729129465073, 61.93301270000000613, 46.70000000109248361 ) ) ;
#3192 = CARTESIAN_POINT ( 'NONE',  ( -13.49542703274178379, -19.04416526290806289, 4.482427507916957765 ) ) ;
#3193 = DIRECTION ( 'NONE',  ( 0.000000000000000000, 1.000000000000000000, -0.000000000000000000 ) ) ;
#3194 = CARTESIAN_POINT ( 'NONE',  ( -19.41254052147348830, -26.35725562635142083, 13.01367750791695777 ) ) ;
#3195 = DIRECTION ( 'NONE',  ( -0.000000000000000000, 1.000000000000000000, -0.000000000000000000 ) ) ;
#3196 = CARTESIAN_POINT ( 'NONE',  ( -7.999999999999986677, 60.00000000000000711, 45.00000000000000000 ) ) ;
#3197 = ADVANCED_FACE ( 'NONE', ( #1056 ), #14296, .T. ) ;
#3198 = B_SPLINE_CURVE_WITH_KNOTS ( 'NONE', 1,
 ( #13501, #5963 ),
 .UNSPECIFIED., .F., .F.,
 ( 2, 2 ),
 ( 0.000000000000000000, 1.000000000000000000 ),
 .UNSPECIFIED. ) ;
#3199 = CARTESIAN_POINT ( 'NONE',  ( 1.461580736456473906, 62.53841926354353120, 46.85000000109246798 ) ) ;
#3200 = DIRECTION ( 'NONE',  ( 1.000000000000000000, 0.000000000000000000, 0.000000000000000000 ) ) ;
#3201 = VECTOR ( 'NONE', #9235, 1000.000000000000000 ) ;
#3202 = DIRECTION ( 'NONE',  ( 1.000000000000000000, -0.000000000000000000, -0.000000000000000000 ) ) ;
#3203 = CARTESIAN_POINT ( 'NONE',  ( 2.066987300000001415, 64.00000000000000000, 46.15000000109247225 ) ) ;
#3204 = DIRECTION ( 'NONE',  ( -1.000000000000000000, 0.000000000000000000, 0.000000000000000000 ) ) ;
#3205 = CARTESIAN_POINT ( 'NONE',  ( -41.00000000000000711, 53.00000000000000711, -45.00000000000000000 ) ) ;
#3206 = DIRECTION ( 'NONE',  ( 1.000000000000000000, 0.000000000000000000, 2.973811673103096679E-16 ) ) ;
#3207 = VERTEX_POINT ( 'NONE', #16153 ) ;
#3208 = ORIENTED_EDGE ( 'NONE', *, *, #12727, .T. ) ;
#3209 = CARTESIAN_POINT ( 'NONE',  ( -8.044165262908093084, -21.95952864787946979, 17.83007249208304046 ) ) ;
#3210 = SURFACE_STYLE_USAGE ( .BOTH. , #13686 ) ;
#3211 = CARTESIAN_POINT ( 'NONE',  ( -10.04416526290808598, -22.49542703274172695, 17.83007249208304046 ) ) ;
#3213 = ORIENTED_EDGE ( 'NONE', *, *, #11832, .T. ) ;
#3212 = ORIENTED_EDGE ( 'NONE', *, *, #1238, .F. ) ;
#3214 = CARTESIAN_POINT ( 'NONE',  ( -17.51566270880201159, -22.35725562635141728, 19.13867750791695954 ) ) ;
#3215 = PRODUCT_RELATED_PRODUCT_CATEGORY ( 'part', '', ( #16315 ) ) ;
#3216 = DIRECTION ( 'NONE',  ( -1.000000000000000000, -0.000000000000000000, -0.000000000000000000 ) ) ;
#3217 = CARTESIAN_POINT ( 'NONE',  ( -20.24501739517664234, -29.00369391078761439, 39.04492750791695954 ) ) ;
#3218 = CARTESIAN_POINT ( 'NONE',  ( -1.461580736456473462, 62.53841926354353120, 48.85000000109246798 ) ) ;
#3219 = CARTESIAN_POINT ( 'NONE',  ( -2.066987300000001415, 63.14382582708705627, 45.60000000109246088 ) ) ;
#3220 = ORIENTED_EDGE ( 'NONE', *, *, #15244, .T. ) ;
#3221 = ORIENTED_EDGE ( 'NONE', *, *, #2297, .F. ) ;
#3222 = CARTESIAN_POINT ( 'NONE',  ( -37.50000000000002842, -0.000000000000000000, -47.50000000000002132 ) ) ;
#3223 = EDGE_LOOP ( 'NONE', ( #5305, #12286, #13981, #2245 ) ) ;
#3224 = EDGE_LOOP ( 'NONE', ( #1461, #3421, #10604, #3377, #7859, #9045, #1956 ) ) ;
#3225 = CARTESIAN_POINT ( 'NONE',  ( 2.066987300000001415, 64.85617417291294373, 48.40000000109247225 ) ) ;
#3226 = CARTESIAN_POINT ( 'NONE',  ( 0.000000000000000000, -6.000000000000000000, 0.000000000000000000 ) ) ;
#3227 = CARTESIAN_POINT ( 'NONE',  ( 1.461580736456473906, 62.53841926354353120, 46.05000000109246372 ) ) ;
#3228 = FACE_OUTER_BOUND ( 'NONE', #8260, .T. ) ;
#3229 = CARTESIAN_POINT ( 'NONE',  ( 2.500000000000001776, 65.03553390593273775, 47.35000000218494165 ) ) ;
#3230 = VERTEX_POINT ( 'NONE', #17522 ) ;
#3232 = VERTEX_POINT ( 'NONE', #8695 ) ;
#3231 = ORIENTED_EDGE ( 'NONE', *, *, #16480, .F. ) ;
#3233 = CARTESIAN_POINT ( 'NONE',  ( -12.95952864787955150, -17.04416526290805933, 14.98242750791695777 ) ) ;
#3234 = DIRECTION ( 'NONE',  ( 0.000000000000000000, 0.000000000000000000, 1.000000000000000000 ) ) ;
#3235 = ORIENTED_EDGE ( 'NONE', *, *, #4338, .F. ) ;
#3236 = VERTEX_POINT ( 'NONE', #13003 ) ;
#3237 = CARTESIAN_POINT ( 'NONE',  ( -15.16482700510262482, -20.99999999999997513, 21.98632249208304046 ) ) ;
#3238 = CARTESIAN_POINT ( 'NONE',  ( -15.16482700510258574, -30.99999999999998224, 6.888677507916956877 ) ) ;
#3239 = CARTESIAN_POINT ( 'NONE',  ( 1.461580736456473684, 65.46158073645646880, 49.25000000109246656 ) ) ;
#3240 = CARTESIAN_POINT ( 'NONE',  ( -41.00000000000000711, 53.00000000000000711, 6.999999999999999112 ) ) ;
#3241 = ORIENTED_EDGE ( 'NONE', *, *, #7586, .T. ) ;
#3242 = CARTESIAN_POINT ( 'NONE',  ( -12.92450931948788906, -26.31681416490114245, 11.48242750791695954 ) ) ;
#3243 = CARTESIAN_POINT ( 'NONE',  ( 44.99999999999998579, 3.000000000000000000, -53.49999999999998579 ) ) ;
#3244 = ORIENTED_EDGE ( 'NONE', *, *, #12564, .F. ) ;
#3245 = CARTESIAN_POINT ( 'NONE',  ( -2.499999999999996003, 62.96446609406726225, 45.25000000000000000 ) ) ;
#3246 = ORIENTED_EDGE ( 'NONE', *, *, #11267, .F. ) ;
#3247 = CARTESIAN_POINT ( 'NONE',  ( -21.50000000000000000, 2.999000000000001442, 32.50000000000000000 ) ) ;
#3248 = CARTESIAN_POINT ( 'NONE',  ( -2.500000000000001776, 65.03553390593273775, 46.74999999999999289 ) ) ;
#3249 = DIRECTION ( 'NONE',  ( -0.000000000000000000, -1.000000000000000000, -0.000000000000000000 ) ) ;
#3250 = DIRECTION ( 'NONE',  ( -0.000000000000000000, -0.000000000000000000, -1.000000000000000000 ) ) ;
#3251 = CONTEXT_DEPENDENT_SHAPE_REPRESENTATION ( #17452, #18967 ) ;
#3252 = PLANE ( 'NONE',  #8645 ) ;
#3253 = FACE_OUTER_BOUND ( 'NONE', #16379, .T. ) ;
#3254 = ADVANCED_FACE ( 'NONE', ( #19004 ), #6757, .T. ) ;
#3255 = ADVANCED_FACE ( 'NONE', ( #11528 ), #8258, .F. ) ;
#3256 = CARTESIAN_POINT ( 'NONE',  ( -11.46040770435012668, -27.78091578003887463, 37.73242750791694533 ) ) ;
#3257 = DIRECTION ( 'NONE',  ( 1.000000000000000000, 0.000000000000000000, -0.000000000000000000 ) ) ;
#3258 = ORIENTED_EDGE ( 'NONE', *, *, #12894, .T. ) ;
#3260 = ADVANCED_FACE ( 'NONE', ( #1014 ), #6880, .T. ) ;
#3259 = CARTESIAN_POINT ( 'NONE',  ( -12.64274437364855252, -28.41254052147347053, 16.95117750791695954 ) ) ;
#3261 = LINE ( 'NONE', #9232, #17730 ) ;
#3262 = ORIENTED_EDGE ( 'NONE', *, *, #888, .F. ) ;
#3263 = CARTESIAN_POINT ( 'NONE',  ( -13.82508104294702100, -18.95583473709188382, 16.95507249208304046 ) ) ;
#3264 = EDGE_CURVE ( 'NONE', #16948, #4790, #17040, .T. ) ;
#3265 = CARTESIAN_POINT ( 'NONE',  ( 2.315774708385941683, 31.32836399182263065, 54.80336399182266405 ) ) ;
#3266 = CARTESIAN_POINT ( 'NONE',  ( -17.51566270880199738, -25.64274437364856496, 14.98632249208304046 ) ) ;
#3267 =( BOUNDED_CURVE ( )  B_SPLINE_CURVE ( 2, ( #4187, #1044, #2999, #19184, #10140, #7314, #7220, #11515, #5751 ),
 .UNSPECIFIED., .F., .F. ) 
 B_SPLINE_CURVE_WITH_KNOTS ( ( 3, 2, 2, 2, 3 ),
 ( 0.7857142857142856984, 0.8035714285714286031, 0.8214285714285712858, 0.8392857142857141906, 0.8571428571428568732 ),
 .UNSPECIFIED. ) 
 CURVE ( )  GEOMETRIC_REPRESENTATION_ITEM ( )  RATIONAL_B_SPLINE_CURVE ( ( 1.000000000000000000, 0.9238795325112867385, 1.000000000000000000, 0.9238795325112867385, 1.000000000000000000, 0.9238795325112867385, 1.000000000000000000, 0.9238795325112877377, 0.9999999999999990008 ) ) 
 REPRESENTATION_ITEM ( '' )  );
#3268 = FILL_AREA_STYLE_COLOUR ( '', #17539 ) ;
#3269 = ORIENTED_EDGE ( 'NONE', *, *, #384, .T. ) ;
#3270 = LINE ( 'NONE', #521, #14377 ) ;
#3271 = ORIENTED_EDGE ( 'NONE', *, *, #13416, .F. ) ;
#3272 = CARTESIAN_POINT ( 'NONE',  ( 24.99999999999999289, -6.000000000000000000, -47.50000000000002132 ) ) ;
#3273 = EDGE_CURVE ( 'NONE', #15565, #12155, #10108, .T. ) ;
#3274 = LINE ( 'NONE', #15136, #13277 ) ;
#3275 = FACE_OUTER_BOUND ( 'NONE', #13101, .T. ) ;
#3276 = PRESENTATION_LAYER_ASSIGNMENT (  '', '', ( #6416 ) ) ;
#3277 = CARTESIAN_POINT ( 'NONE',  ( -13.50000000000003908, 20.01992244580436164, 66.11180553784085134 ) ) ;
#3278 = DIRECTION ( 'NONE',  ( 1.000000000000000000, 0.000000000000000000, 0.000000000000000000 ) ) ;
#3279 = EDGE_CURVE ( 'NONE', #856, #3523, #9719, .T. ) ;
#3280 =( LENGTH_UNIT ( ) NAMED_UNIT ( * ) SI_UNIT ( .MILLI., .METRE. ) );
#3281 = DIRECTION ( 'NONE',  ( 1.000000000000000000, 0.000000000000000000, -0.000000000000000000 ) ) ;
#3282 = ORIENTED_EDGE ( 'NONE', *, *, #7108, .T. ) ;
#3283 = DIRECTION ( 'NONE',  ( 1.000000000000000000, 0.000000000000000000, 0.000000000000000000 ) ) ;
#3284 = CARTESIAN_POINT ( 'NONE',  ( -13.49542703274178379, -19.04416526290806289, 14.98242750791695777 ) ) ;
#3285 = VECTOR ( 'NONE', #5821, 1000.000000000000000 ) ;
#3286 = CARTESIAN_POINT ( 'NONE',  ( -1.767766952966370209, 65.76776695296638309, 45.20000000218494307 ) ) ;
#3287 = CARTESIAN_POINT ( 'NONE',  ( -18.78091578003892081, -20.46040770435013556, 16.08007249208304401 ) ) ;
#3288 = ADVANCED_FACE ( 'NONE', ( #18518 ), #8557, .F. ) ;
#3289 = EDGE_CURVE ( 'NONE', #14577, #8458, #13150, .T. ) ;
#3290 = CARTESIAN_POINT ( 'NONE',  ( 3.796994071234847710E-16, 61.93301269999999903, 45.95000000109246940 ) ) ;
#3291 = CARTESIAN_POINT ( 'NONE',  ( -10.75228648362910100, -26.64274437364854009, 16.51367750791695954 ) ) ;
#3292 = ADVANCED_FACE ( 'NONE', ( #4250 ), #17581, .F. ) ;
#3293 = CARTESIAN_POINT ( 'NONE',  ( -24.00000000000000000, 110.0000000000000000, 30.00000000000000000 ) ) ;
#3294 = CARTESIAN_POINT ( 'NONE',  ( -12.64274437364855252, -28.41254052147347053, 22.20117750791695599 ) ) ;
#3295 = LINE ( 'NONE', #448, #8119 ) ;
#3296 = LINE ( 'NONE', #4672, #9754 ) ;
#3297 = EDGE_CURVE ( 'NONE', #574, #8644, #10230, .T. ) ;
#3298 = CARTESIAN_POINT ( 'NONE',  ( -1.461580736456473462, 62.53841926354353120, 49.05000000109247082 ) ) ;
#3299 = PLANE ( 'NONE',  #14340 ) ;
#3300 = DIRECTION ( 'NONE',  ( 1.000000000000000000, 0.000000000000000000, 0.000000000000000000 ) ) ;
#3301 = VECTOR ( 'NONE', #12288, 1000.000000000000000 ) ;
#3302 = CARTESIAN_POINT ( 'NONE',  ( 1.767766952966369987, 65.76776695296638309, 48.20000000218494307 ) ) ;
#3303 = CARTESIAN_POINT ( 'NONE',  ( -1.265664690411616068E-16, 66.06698730000000808, 47.95000000109246940 ) ) ;
#3304 = CARTESIAN_POINT ( 'NONE',  ( -50.00000000000002132, 115.0000000000000000, 37.49999999999997868 ) ) ;
#3305 = ORIENTED_EDGE ( 'NONE', *, *, #11039, .T. ) ;
#3306 = EDGE_LOOP ( 'NONE', ( #5461, #1780, #9762, #9494 ) ) ;
#3307 = CARTESIAN_POINT ( 'NONE',  ( -17.04047135212050890, -17.04416526290807710, 32.26757249208304046 ) ) ;
#3308 = CARTESIAN_POINT ( 'NONE',  ( -20.04416526290809131, -22.82508104294700502, 5.142572492083039570 ) ) ;
#3309 = ORIENTED_EDGE ( 'NONE', *, *, #6175, .T. ) ;
#3310 = EDGE_CURVE ( 'NONE', #15535, #15167, #1270, .T. ) ;
#3311 = CARTESIAN_POINT ( 'NONE',  ( -18.04416526290808420, -24.63902057219074493, 13.23242750791696132 ) ) ;
#3312 = EDGE_CURVE ( 'NONE', #13315, #11055, #8650, .T. ) ;
#3313 = DIRECTION ( 'NONE',  ( -0.000000000000000000, 1.000000000000000000, -0.000000000000000000 ) ) ;
#3314 = CARTESIAN_POINT ( 'NONE',  ( -15.16482700510264436, -16.99999999999997868, 16.73632249208304046 ) ) ;
#3315 = VECTOR ( 'NONE', #19336, 1000.000000000000000 ) ;
#3316 = AXIS2_PLACEMENT_3D ( 'NONE', #5169, #8214, #5082 ) ;
#3317 = CARTESIAN_POINT ( 'NONE',  ( -2.500000000000001776, 64.00000000000000000, 49.99999999999999289 ) ) ;
#3318 = CARTESIAN_POINT ( 'NONE',  ( 1.461580736456473684, 65.46158073645646880, 45.25000000109247367 ) ) ;
#3319 = ORIENTED_EDGE ( 'NONE', *, *, #4999, .F. ) ;
#3320 = EDGE_LOOP ( 'NONE', ( #3991, #6363, #14479, #13024 ) ) ;
#3321 = LINE ( 'NONE', #15087, #14393 ) ;
#3322 = LINE ( 'NONE', #18424, #6036 ) ;
#3323 = ORIENTED_EDGE ( 'NONE', *, *, #13137, .T. ) ;
#3324 = DIRECTION ( 'NONE',  ( 0.000000000000000000, 0.000000000000000000, 1.000000000000000000 ) ) ;
#3325 = DIRECTION ( 'NONE',  ( -1.000000000000000000, 0.000000000000000000, -0.000000000000000000 ) ) ;
#3326 = LINE ( 'NONE', #13701, #4435 ) ;
#3327 = APPLICATION_CONTEXT ( 'automotive_design' ) ;
#3328 = DIRECTION ( 'NONE',  ( 0.000000000000000000, -1.000000000000000000, 0.000000000000000000 ) ) ;
#3329 = AXIS2_PLACEMENT_3D ( 'NONE', #3804, #5460, #14100 ) ;
#3330 = VECTOR ( 'NONE', #7296, 1000.000000000000000 ) ;
#3331 = CARTESIAN_POINT ( 'NONE',  ( 1.753982408753060440, -43.60761626555502346, 3.000000000000000000 ) ) ;
#3332 = ORIENTED_EDGE ( 'NONE', *, *, #9838, .T. ) ;
#3334 = ORIENTED_EDGE ( 'NONE', *, *, #5808, .T. ) ;
#3333 = ORIENTED_EDGE ( 'NONE', *, *, #12131, .F. ) ;
#3335 = CARTESIAN_POINT ( 'NONE',  ( -17.04047135212043784, -30.95583473709190159, 17.60742750791695954 ) ) ;
#3336 = ORIENTED_EDGE ( 'NONE', *, *, #9928, .F. ) ;
#3337 = ORIENTED_EDGE ( 'NONE', *, *, #1816, .F. ) ;
#3338 = ADVANCED_FACE ( 'NONE', ( #13991 ), #18868, .F. ) ;
#3339 = CARTESIAN_POINT ( 'NONE',  ( -12.04416526290808420, -23.03132541760398766, 23.08007249208304401 ) ) ;
#3340 = CARTESIAN_POINT ( 'NONE',  ( -15.16482700510258574, -30.99999999999998224, 17.38867750791695599 ) ) ;
#3341 = CARTESIAN_POINT ( 'NONE',  ( -0.8561741729129461742, 66.06698730000000808, 48.60000000109246798 ) ) ;
#3342 = CARTESIAN_POINT ( 'NONE',  ( -41.00000000000000711, 110.0000000000000000, -24.49999999999999645 ) ) ;
#3343 = ORIENTED_EDGE ( 'NONE', *, *, #327, .T. ) ;
#3344 = CARTESIAN_POINT ( 'NONE',  ( -18.04416526290808420, -24.63902057219074493, 18.48242750791695954 ) ) ;
#3345 = VECTOR ( 'NONE', #13543, 1000.000000000000000 ) ;
#3346 = PLANE ( 'NONE',  #10336 ) ;
#3347 = VERTEX_POINT ( 'NONE', #12869 ) ;
#3348 = AXIS2_PLACEMENT_3D ( 'NONE', #18480, #3566, #5714 ) ;
#3349 = DIRECTION ( 'NONE',  ( 1.000000000000000000, 0.000000000000000000, 0.000000000000000000 ) ) ;
#3350 = ORIENTED_EDGE ( 'NONE', *, *, #13689, .T. ) ;
#3351 = FILL_AREA_STYLE_COLOUR ( '', #16640 ) ;
#3352 = FACE_BOUND ( 'NONE', #3535, .T. ) ;
#3353 = LINE ( 'NONE', #308, #9389 ) ;
#3354 = LINE ( 'NONE', #13927, #4875 ) ;
#3355 = CARTESIAN_POINT ( 'NONE',  ( 1.461580736456473906, 62.53841926354353120, 49.05000000109247082 ) ) ;
#3356 = LINE ( 'NONE', #9321, #16496 ) ;
#3357 = DIRECTION ( 'NONE',  ( 0.000000000000000000, 1.000000000000000000, 0.000000000000000000 ) ) ;
#3358 = CARTESIAN_POINT ( 'NONE',  ( -18.53959229564986799, -20.21908421996107563, 35.10742750791694533 ) ) ;
#3359 = PLANE ( 'NONE',  #14258 ) ;
#3360 = ORIENTED_EDGE ( 'NONE', *, *, #377, .F. ) ;
#3361 = CARTESIAN_POINT ( 'NONE',  ( -18.78091578003889950, -27.53959229564985378, 18.04492750791695954 ) ) ;
#3362 = AXIS2_PLACEMENT_3D ( 'NONE', #9801, #14504, #15795 ) ;
#3363 = LINE ( 'NONE', #3645, #529 ) ;
#3364 = ORIENTED_EDGE ( 'NONE', *, *, #6641, .F. ) ;
#3365 = CARTESIAN_POINT ( 'NONE',  ( -18.53959229564982536, -27.78091578003890660, 14.76757249208303691 ) ) ;
#3366 = CARTESIAN_POINT ( 'NONE',  ( -12.92450931948790149, -21.68318583509881137, 12.14257249208304223 ) ) ;
#3367 = ORIENTED_EDGE ( 'NONE', *, *, #4746, .T. ) ;
#3368 = DIRECTION ( 'NONE',  ( -1.000000000000000000, 0.000000000000000000, -0.000000000000000000 ) ) ;
#3369 = ORIENTED_EDGE ( 'NONE', *, *, #9870, .F. ) ;
#3370 = DIRECTION ( 'NONE',  ( -1.047444401652940007E-14, -0.7071067811865495711, 0.7071067811865454633 ) ) ;
#3371 = LINE ( 'NONE', #524, #2979 ) ;
#3372 = CARTESIAN_POINT ( 'NONE',  ( -41.00000000000000711, 110.0000000000000000, -5.000000000000004441 ) ) ;
#3373 = FACE_BOUND ( 'NONE', #5404, .T. ) ;
#3374 =( LENGTH_UNIT ( ) NAMED_UNIT ( * ) SI_UNIT ( .MILLI., .METRE. ) );
#3375 = CARTESIAN_POINT ( 'NONE',  ( 32.50000000000000000, 0.000000000000000000, -25.00000000000001421 ) ) ;
#3376 = LINE ( 'NONE', #3076, #14576 ) ;
#3377 = ORIENTED_EDGE ( 'NONE', *, *, #19080, .T. ) ;
#3378 = DIRECTION ( 'NONE',  ( 1.000000000000000000, 0.000000000000000000, 0.000000000000000000 ) ) ;
#3379 = CARTESIAN_POINT ( 'NONE',  ( -19.99999999999999645, -23.83517299489738051, 13.45117750791695777 ) ) ;
#3380 = CARTESIAN_POINT ( 'NONE',  ( -2.500000000000001776, 65.03553390593273775, 46.05000000218494449 ) ) ;
#3381 = EDGE_CURVE ( 'NONE', #18025, #17238, #913, .T. ) ;
#3382 = CARTESIAN_POINT ( 'NONE',  ( -19.24771351637086880, -26.64274437364857206, 20.23632249208304046 ) ) ;
#3383 = CARTESIAN_POINT ( 'NONE',  ( 24.99999999999998579, -6.000000000000000000, 47.49999999999997868 ) ) ;
#3384 = CARTESIAN_POINT ( 'NONE',  ( -9.955834737091912245, -22.82508104294696594, 15.85742750791695777 ) ) ;
#3385 = DIRECTION ( 'NONE',  ( -1.000000000000000000, 0.000000000000000000, -0.000000000000000000 ) ) ;
#3386 = CARTESIAN_POINT ( 'NONE',  ( -18.53959229564986799, -20.21908421996107563, 19.35742750791695954 ) ) ;
#3387 = CARTESIAN_POINT ( 'NONE',  ( 44.99999999999998579, -1.285879139104706187E-16, -54.99999999999998579 ) ) ;
#3388 = FACE_BOUND ( 'NONE', #10760, .T. ) ;
#3389 = CARTESIAN_POINT ( 'NONE',  ( -2.066987300000001859, 64.85617417291294373, 47.30000000109247082 ) ) ;
#3390 = DIRECTION ( 'NONE',  ( 1.000000000000000000, -0.000000000000000000, -0.000000000000000000 ) ) ;
#3391 = LINE ( 'NONE', #9362, #836 ) ;
#3392 = CARTESIAN_POINT ( 'NONE',  ( -2.066987300000001859, 64.85617417291294373, 48.10000000109246798 ) ) ;
#3393 = CARTESIAN_POINT ( 'NONE',  ( 34.99999999999999289, 0.000000000000000000, 47.49999999999997868 ) ) ;
#3394 = AXIS2_PLACEMENT_3D ( 'NONE', #16927, #17117, #547 ) ;
#3395 = EDGE_CURVE ( 'NONE', #9366, #7944, #9917, .T. ) ;
#3396 = EDGE_CURVE ( 'NONE', #7331, #4488, #6019, .T. ) ;
#3397 = VERTEX_POINT ( 'NONE', #11978 ) ;
#3398 = EDGE_LOOP ( 'NONE', ( #9677, #5414, #14418, #16563 ) ) ;
#3399 = ADVANCED_FACE ( 'NONE', ( #16399 ), #5816, .F. ) ;
#3400 = CARTESIAN_POINT ( 'NONE',  ( -15.16482700510264436, -16.99999999999997868, 32.48632249208304046 ) ) ;
#3401 = CARTESIAN_POINT ( 'NONE',  ( -13.82508104294702100, -18.95583473709188382, 11.70507249208304046 ) ) ;
#3402 = ORIENTED_EDGE ( 'NONE', *, *, #4719, .F. ) ;
#3403 = CARTESIAN_POINT ( 'NONE',  ( -16.35725562635142794, -21.31951028609535470, 24.82617750791696309 ) ) ;
#3404 = CARTESIAN_POINT ( 'NONE',  ( -41.00000000000000711, 110.0000000000000000, -12.50000000000000000 ) ) ;
#3405 = CARTESIAN_POINT ( 'NONE',  ( -7.999999999999996447, -23.83517299489733432, 23.29882249208304046 ) ) ;
#3406 = CARTESIAN_POINT ( 'NONE',  ( -0.8561741729129461742, 66.06698729999999387, 47.00000000109247367 ) ) ;
#3407 = CARTESIAN_POINT ( 'NONE',  ( -2.066987300000001415, 64.00000000000000000, 47.15000000109247225 ) ) ;
#3408 = ORIENTED_EDGE ( 'NONE', *, *, #1816, .T. ) ;
#3409 = EDGE_LOOP ( 'NONE', ( #14733, #16648 ) ) ;
#3410 = AXIS2_PLACEMENT_3D ( 'NONE', #4278, #11806, #1335 ) ;
#3411 = DIRECTION ( 'NONE',  ( -0.000000000000000000, -1.000000000000000000, -0.000000000000000000 ) ) ;
#3412 = DIRECTION ( 'NONE',  ( -0.000000000000000000, -0.000000000000000000, -1.000000000000000000 ) ) ;
#3413 = CARTESIAN_POINT ( 'NONE',  ( -1.265664690411616068E-16, 66.06698730000000808, 48.55000000109247082 ) ) ;
#3414 = CARTESIAN_POINT ( 'NONE',  ( -40.00000000000000711, 53.00000000000000711, 21.00000000000000000 ) ) ;
#3415 = CARTESIAN_POINT ( 'NONE',  ( -0.8561741729129465073, 61.93301270000000613, 45.10000000109246798 ) ) ;
#3416 = CARTESIAN_POINT ( 'NONE',  ( -25.00000000000000000, 53.00000000000000711, -12.49999999999999645 ) ) ;
#3417 = AXIS2_PLACEMENT_3D ( 'NONE', #12133, #8901, #4206 ) ;
#3418 = EDGE_CURVE ( 'NONE', #4550, #8057, #11780, .T. ) ;
#3419 = DIRECTION ( 'NONE',  ( 0.000000000000000000, 1.000000000000000000, -0.000000000000000000 ) ) ;
#3420 = ORIENTED_EDGE ( 'NONE', *, *, #2948, .F. ) ;
#3422 = EDGE_LOOP ( 'NONE', ( #2521, #2243, #13517, #11831 ) ) ;
#3421 = ORIENTED_EDGE ( 'NONE', *, *, #9621, .F. ) ;
#3423 = CARTESIAN_POINT ( 'NONE',  ( -7.955834737091916686, -22.28918265808470522, 31.60742750791695244 ) ) ;
#3424 = AXIS2_PLACEMENT_3D ( 'NONE', #11166, #3542, #6681 ) ;
#3425 = SHAPE_REPRESENTATION_RELATIONSHIP ( 'NONE' , 'NONE' ,  #13906, #571 ) ;
#3426 = EDGE_LOOP ( 'NONE', ( #5112, #12435, #9961, #10168 ) ) ;
#3427 = ORIENTED_EDGE ( 'NONE', *, *, #16911, .T. ) ;
#3428 = CARTESIAN_POINT ( 'NONE',  ( -13.35725562635141195, -26.51566270880198672, 29.42382249208304401 ) ) ;
#3429 = CARTESIAN_POINT ( 'NONE',  ( -12.95952864787955150, -17.04416526290805933, 20.23242750791695954 ) ) ;
#3430 = CARTESIAN_POINT ( 'NONE',  ( -1.461580736456473906, 65.46158073645646880, 47.05000000109247082 ) ) ;
#3431 = CARTESIAN_POINT ( 'NONE',  ( -44.99999999999998579, 3.000000000000000000, -53.50000000000000000 ) ) ;
#3432 = ORIENTED_EDGE ( 'NONE', *, *, #7464, .F. ) ;
#3433 = CARTESIAN_POINT ( 'NONE',  ( -13.64274437364856141, -26.68048971390460622, 11.70117750791696132 ) ) ;
#3434 = AXIS2_PLACEMENT_3D ( 'NONE', #12694, #18698, #18885 ) ;
#3435 = DIRECTION ( 'NONE',  ( 1.000000000000000000, 0.000000000000000000, -5.782411586589357392E-17 ) ) ;
#3436 = ORIENTED_EDGE ( 'NONE', *, *, #1878, .T. ) ;
#3437 = DIRECTION ( 'NONE',  ( 0.000000000000000000, 1.000000000000000000, -1.320393690296331133E-15 ) ) ;
#3438 = ORIENTED_EDGE ( 'NONE', *, *, #5281, .F. ) ;
#3439 = DIRECTION ( 'NONE',  ( 0.000000000000000000, 1.000000000000000000, -1.320393690296331133E-15 ) ) ;
#3440 = DIRECTION ( 'NONE',  ( 0.000000000000000000, 0.000000000000000000, -1.000000000000000000 ) ) ;
#3441 = CARTESIAN_POINT ( 'NONE',  ( -2.499999999999996003, 62.96446609406726225, 45.25000000000000000 ) ) ;
#3442 = PLANE ( 'NONE',  #6856 ) ;
#3443 = PLANE ( 'NONE',  #1730 ) ;
#3444 = VECTOR ( 'NONE', #1201, 1000.000000000000114 ) ;
#3445 = CARTESIAN_POINT ( 'NONE',  ( -25.00000000000000711, 53.00000000000000711, 8.000000000000000000 ) ) ;
#3446 = AXIS2_PLACEMENT_3D ( 'NONE', #2536, #8518, #14493 ) ;
#3447 = EDGE_CURVE ( 'NONE', #16356, #12614, #13465, .T. ) ;
#3448 = FACE_OUTER_BOUND ( 'NONE', #7421, .T. ) ;
#3449 = DIRECTION ( 'NONE',  ( -1.156482317317871478E-16, 1.000000000000000000, 0.000000000000000000 ) ) ;
#3450 = DIRECTION ( 'NONE',  ( 1.000000000000000000, 0.000000000000000000, 0.000000000000000000 ) ) ;
#3451 = DIRECTION ( 'NONE',  ( -0.000000000000000000, -0.000000000000000000, -1.000000000000000000 ) ) ;
#3452 = ORIENTED_EDGE ( 'NONE', *, *, #14948, .F. ) ;
#3453 = CARTESIAN_POINT ( 'NONE',  ( -13.82508104294698192, -29.04416526290806644, 32.91992750791695954 ) ) ;
#3454 = PLANE ( 'NONE',  #2098 ) ;
#3455 = VERTEX_POINT ( 'NONE', #16701 ) ;
#3456 = AXIS2_PLACEMENT_3D ( 'NONE', #12521, #274, #18123 ) ;
#3457 = CARTESIAN_POINT ( 'NONE',  ( -19.41254052147350961, -21.64274437364857562, 15.86132249208304223 ) ) ;
#3458 = EDGE_CURVE ( 'NONE', #10251, #10640, #17772, .T. ) ;
#3459 = AXIS2_PLACEMENT_3D ( 'NONE', #693, #6677, #16627 ) ;
#3460 = CARTESIAN_POINT ( 'NONE',  ( -14.36097942780925685, -20.95583473709189093, 22.20507249208304401 ) ) ;
#3461 = LINE ( 'NONE', #18569, #941 ) ;
#3462 = ORIENTED_EDGE ( 'NONE', *, *, #12015, .F. ) ;
#3463 = MECHANICAL_DESIGN_GEOMETRIC_PRESENTATION_REPRESENTATION (  '', ( #7849 ), #355 ) ;
#3464 = LINE ( 'NONE', #12378, #9375 ) ;
#3465 = ORIENTED_EDGE ( 'NONE', *, *, #7972, .F. ) ;
#3466 = CARTESIAN_POINT ( 'NONE',  ( 0.000000000000000000, 115.0000000000000000, 0.000000000000000000 ) ) ;
#3467 = FACE_OUTER_BOUND ( 'NONE', #17184, .T. ) ;
#3468 = CARTESIAN_POINT ( 'NONE',  ( -1.767766952966370209, 65.76776695296638309, 46.00000000218494733 ) ) ;
#3469 = AXIS2_PLACEMENT_3D ( 'NONE', #11925, #11718, #14779 ) ;
#3470 = EDGE_CURVE ( 'NONE', #982, #17652, #9398, .T. ) ;
#3471 = DIRECTION ( 'NONE',  ( 0.000000000000000000, -1.000000000000000000, 0.000000000000000000 ) ) ;
#3472 = AXIS2_PLACEMENT_3D ( 'NONE', #3916, #5581, #12924 ) ;
#3473 = CARTESIAN_POINT ( 'NONE',  ( -1.530808498934192803E-16, 66.50000000000000000, 45.00000000000000000 ) ) ;
#3474 = DIRECTION ( 'NONE',  ( -0.000000000000000000, -1.000000000000000000, -0.000000000000000000 ) ) ;
#3475 = AXIS2_PLACEMENT_3D ( 'NONE', #18910, #12638, #8415 ) ;
#3476 = ORIENTED_EDGE ( 'NONE', *, *, #6386, .F. ) ;
#3477 = VECTOR ( 'NONE', #12382, 1000.000000000000000 ) ;
#3478 = CARTESIAN_POINT ( 'NONE',  ( -9.999999999999994671, -24.16482700510257686, 10.82617750791695777 ) ) ;
#3479 = CARTESIAN_POINT ( 'NONE',  ( 1.767766952966369987, 65.76776695296638309, 47.40000000218494591 ) ) ;
#3480 = CARTESIAN_POINT ( 'NONE',  ( -15.16482700510263371, -18.99999999999997868, 21.98632249208304401 ) ) ;
#3481 = VECTOR ( 'NONE', #17234, 1000.000000000000000 ) ;
#3482 = CARTESIAN_POINT ( 'NONE',  ( 24.99999999999998579, 107.3545527679194436, 47.49999999999997868 ) ) ;
#3483 = CARTESIAN_POINT ( 'NONE',  ( -18.53959229564986799, -20.21908421996107563, 19.35742750791695599 ) ) ;
#3484 = DIRECTION ( 'NONE',  ( -1.156482317317871478E-16, 1.000000000000000000, 0.000000000000000000 ) ) ;
#3485 = CARTESIAN_POINT ( 'NONE',  ( -18.78091578003889595, -27.53959229564985023, 23.29492750791695954 ) ) ;
#3486 = DIRECTION ( 'NONE',  ( -1.541976423090495880E-16, 0.000000000000000000, 1.000000000000000000 ) ) ;
#3487 = CARTESIAN_POINT ( 'NONE',  ( -17.64274437364858983, -19.75228648362910633, 32.04882249208304046 ) ) ;
#3488 = CARTESIAN_POINT ( 'NONE',  ( 3.796994071234847710E-16, 61.93301269999999903, 46.75000000109246656 ) ) ;
#3489 = DIRECTION ( 'NONE',  ( 0.000000000000000000, 0.000000000000000000, -1.000000000000000000 ) ) ;
#3490 = DIRECTION ( 'NONE',  ( 0.000000000000000000, 0.000000000000000000, 1.000000000000000000 ) ) ;
#3491 = VECTOR ( 'NONE', #6146, 1000.000000000000000 ) ;
#3492 = LINE ( 'NONE', #9466, #2708 ) ;
#3493 = CARTESIAN_POINT ( 'NONE',  ( -1.461580736456473462, 62.53841926354353120, 47.45000000109246230 ) ) ;
#3494 = EDGE_CURVE ( 'NONE', #2269, #15646, #4648, .T. ) ;
#3495 = EDGE_CURVE ( 'NONE', #4095, #2670, #5335, .T. ) ;
#3496 = FACE_OUTER_BOUND ( 'NONE', #11086, .T. ) ;
#3497 =( BOUNDED_CURVE ( )  B_SPLINE_CURVE ( 2, ( #10139, #14281, #3987, #12710, #3803, #9769, #2510, #9856, #8588 ),
 .UNSPECIFIED., .F., .F. ) 
 B_SPLINE_CURVE_WITH_KNOTS ( ( 3, 2, 2, 2, 3 ),
 ( 0.2142857142857141350, 0.2321428571428569565, 0.2499999999999997224, 0.2678571428571425161, 0.2857142857142853098 ),
 .UNSPECIFIED. ) 
 CURVE ( )  GEOMETRIC_REPRESENTATION_ITEM ( )  RATIONAL_B_SPLINE_CURVE ( ( 1.000000000000000666, 0.9238795325112861834, 1.000000000000000000, 0.9238795325112867385, 1.000000000000000000, 0.9238795325112867385, 1.000000000000000000, 0.9238795325112884038, 0.9999999999999983347 ) ) 
 REPRESENTATION_ITEM ( '' )  );
#3498 =( GEOMETRIC_REPRESENTATION_CONTEXT ( 3 ) GLOBAL_UNCERTAINTY_ASSIGNED_CONTEXT ( ( #10814 ) ) GLOBAL_UNIT_ASSIGNED_CONTEXT ( ( #17192, #2286, #12761 ) ) REPRESENTATION_CONTEXT ( 'NONE', 'WORKASPACE' ) );
#3499 = ORIENTED_EDGE ( 'NONE', *, *, #13062, .F. ) ;
#3500 = ORIENTED_EDGE ( 'NONE', *, *, #16011, .F. ) ;
#3501 = CARTESIAN_POINT ( 'NONE',  ( -20.00369391078757886, -29.24501739517668142, 35.76757249208303335 ) ) ;
#3502 = EDGE_CURVE ( 'NONE', #5079, #1798, #16502, .T. ) ;
#3503 = CARTESIAN_POINT ( 'NONE',  ( -9.955834737091903364, -25.17491895705295235, 13.01757249208304223 ) ) ;
#3504 = ORIENTED_EDGE ( 'NONE', *, *, #9649, .T. ) ;
#3505 = CARTESIAN_POINT ( 'NONE',  ( -17.95583473709191580, -23.03132541760400898, 24.16992750791696309 ) ) ;
#3506 = DIRECTION ( 'NONE',  ( 1.000000000000000000, -0.000000000000000000, -0.000000000000000000 ) ) ;
#3507 = EDGE_CURVE ( 'NONE', #4220, #13466, #10405, .T. ) ;
#3508 = CARTESIAN_POINT ( 'NONE',  ( -16.71081734191520596, -31.04416526290808065, 24.83007249208304046 ) ) ;
#3509 = VECTOR ( 'NONE', #3053, 1000.000000000000000 ) ;
#3510 = CARTESIAN_POINT ( 'NONE',  ( 3.796994071234847710E-16, 61.93301269999999903, 44.95000000109246940 ) ) ;
#3511 = CARTESIAN_POINT ( 'NONE',  ( -1.461580736456473906, 65.46158073645646880, 46.25000000109247367 ) ) ;
#3512 = ORIENTED_EDGE ( 'NONE', *, *, #10326, .F. ) ;
#3513 = VERTEX_POINT ( 'NONE', #14833 ) ;
#3514 = VECTOR ( 'NONE', #582, 1000.000000000000114 ) ;
#3515 = CARTESIAN_POINT ( 'NONE',  ( 1.035533905932738197, 66.50000000000000000, 45.85000000218494165 ) ) ;
#3516 = DIRECTION ( 'NONE',  ( -0.000000000000000000, -0.000000000000000000, -1.000000000000000000 ) ) ;
#3517 = FACE_OUTER_BOUND ( 'NONE', #7642, .T. ) ;
#3518 = LINE ( 'NONE', #12706, #18159 ) ;
#3519 = EDGE_CURVE ( 'NONE', #7431, #4122, #10990, .T. ) ;
#3520 = CARTESIAN_POINT ( 'NONE',  ( -1.461580736456473906, 65.46158073645646880, 45.65000000109247225 ) ) ;
#3521 = LINE ( 'NONE', #7841, #18197 ) ;
#3522 = CARTESIAN_POINT ( 'NONE',  ( -1.530808498934192803E-16, 66.50000000000000000, 47.50000000218494023 ) ) ;
#3523 = VERTEX_POINT ( 'NONE', #14935 ) ;
#3524 = EDGE_CURVE ( 'NONE', #12231, #11212, #6213, .T. ) ;
#3525 = ORIENTED_EDGE ( 'NONE', *, *, #15477, .F. ) ;
#3526 = CARTESIAN_POINT ( 'NONE',  ( -14.83517299489740715, -16.99999999999997868, 30.51367750791695954 ) ) ;
#3527 = ORIENTED_EDGE ( 'NONE', *, *, #10674, .T. ) ;
#3528 = VERTEX_POINT ( 'NONE', #7474 ) ;
#3529 = CARTESIAN_POINT ( 'NONE',  ( -18.04416526290808775, -23.36097942780924441, 36.64257249208304756 ) ) ;
#3530 = CARTESIAN_POINT ( 'NONE',  ( -17.04047135212043784, -30.95583473709190159, 22.85742750791695599 ) ) ;
#3531 = CARTESIAN_POINT ( 'NONE',  ( -1.265664690411616068E-16, 66.06698730000000808, 49.35000000109246798 ) ) ;
#3532 = CARTESIAN_POINT ( 'NONE',  ( 43.49999999999997868, 2.999000000000001442, -52.50000000000002132 ) ) ;
#3533 = ORIENTED_EDGE ( 'NONE', *, *, #656, .T. ) ;
#3534 = CARTESIAN_POINT ( 'NONE',  ( -12.48433729119798130, -25.64274437364855075, 37.51367750791695954 ) ) ;
#3535 = EDGE_LOOP ( 'NONE', ( #10998, #6507, #12058, #6157 ) ) ;
#3536 = EDGE_CURVE ( 'NONE', #5700, #574, #13446, .T. ) ;
#3537 = ADVANCED_FACE ( 'NONE', ( #1606 ), #7581, .T. ) ;
#3538 = LINE ( 'NONE', #9507, #17512 ) ;
#3539 = VERTEX_POINT ( 'NONE', #18075 ) ;
#3540 = LINE ( 'NONE', #6486, #16321 ) ;
#3541 = FACE_BOUND ( 'NONE', #7383, .T. ) ;
#3542 = DIRECTION ( 'NONE',  ( -0.000000000000000000, -1.000000000000000000, -0.000000000000000000 ) ) ;
#3543 = DIRECTION ( 'NONE',  ( 0.000000000000000000, 0.000000000000000000, -1.000000000000000000 ) ) ;
#3544 = CARTESIAN_POINT ( 'NONE',  ( -1.461580736456473906, 65.46158073645646880, 47.85000000109246798 ) ) ;
#3545 = ITEM_DEFINED_TRANSFORMATION ( 'NONE', 'NONE', #9849,  #1791 ) ;
#3546 = EDGE_CURVE ( 'NONE', #17266, #513, #18175, .T. ) ;
#3547 = CARTESIAN_POINT ( 'NONE',  ( -2.500000000000001776, 64.00000000000000000, 49.30000000218494449 ) ) ;
#3548 = DIRECTION ( 'NONE',  ( -0.000000000000000000, 1.000000000000000000, -0.000000000000000000 ) ) ;
#3549 = DIRECTION ( 'NONE',  ( 0.000000000000000000, -1.000000000000000000, 0.000000000000000000 ) ) ;
#3550 = DIRECTION ( 'NONE',  ( -0.5000000000000051070, 0.000000000000000000, 0.8660254037844355990 ) ) ;
#3551 = ORIENTED_EDGE ( 'NONE', *, *, #387, .T. ) ;
#3552 = CARTESIAN_POINT ( 'NONE',  ( -15.16482700510259640, -28.99999999999998224, 33.13867750791696665 ) ) ;
#3553 = LINE ( 'NONE', #7774, #7402 ) ;
#3554 = ORIENTED_EDGE ( 'NONE', *, *, #16920, .T. ) ;
#3555 = CARTESIAN_POINT ( 'NONE',  ( -10.58745947852648328, -26.35725562635138530, 34.23632249208304046 ) ) ;
#3556 = ADVANCED_FACE ( 'NONE', ( #8743 ), #14732, .T. ) ;
#3557 = CARTESIAN_POINT ( 'NONE',  ( -12.31951028609536536, -25.35725562635139596, 18.48632249208304401 ) ) ;
#3558 = EDGE_LOOP ( 'NONE', ( #10549, #14712, #6356, #14505, #17843, #2544, #4769, #3309, #10055, #12014, #9614, #182, #6932, #5407, #8428 ) ) ;
#3559 = CARTESIAN_POINT ( 'NONE',  ( -41.00000000000000711, 110.0000000000000000, 27.50000000000000000 ) ) ;
#3560 = ORIENTED_EDGE ( 'NONE', *, *, #19080, .F. ) ;
#3561 = CARTESIAN_POINT ( 'NONE',  ( -0.1250000000000104083, 27.16170093578836031, 58.97002704785691662 ) ) ;
#3562 = DIRECTION ( 'NONE',  ( 0.000000000000000000, 0.000000000000000000, 1.000000000000000000 ) ) ;
#3563 = CARTESIAN_POINT ( 'NONE',  ( 0.000000000000000000, 64.00000000000000000, 49.99999999999999289 ) ) ;
#3564 = CARTESIAN_POINT ( 'NONE',  ( -1.040834085586084257E-14, 25.49999999999998934, 52.50000000000000000 ) ) ;
#3565 = CARTESIAN_POINT ( 'NONE',  ( 4.999999999999999112, 4.250000000000000000, 0.000000000000000000 ) ) ;
#3566 = DIRECTION ( 'NONE',  ( 0.000000000000000000, -1.000000000000000000, 0.000000000000000000 ) ) ;
#3567 = CARTESIAN_POINT ( 'NONE',  ( -35.00000000000002132, -6.000000000000000000, -47.50000000000002132 ) ) ;
#3568 = UNCERTAINTY_MEASURE_WITH_UNIT (LENGTH_MEASURE( 1.000000000000000082E-05 ), #7762, 'distance_accuracy_value', 'NONE');
#3569 = ORIENTED_EDGE ( 'NONE', *, *, #7811, .F. ) ;
#3570 = CARTESIAN_POINT ( 'NONE',  ( -15.16482700510259640, -28.99999999999998224, 38.38867750791695954 ) ) ;
#3571 = EDGE_CURVE ( 'NONE', #4981, #12140, #3461, .T. ) ;
#3572 = CARTESIAN_POINT ( 'NONE',  ( -2.500000000000001776, 64.00000000000000000, 46.10000000218494165 ) ) ;
#3573 = CARTESIAN_POINT ( 'NONE',  ( -19.95583473709190514, -25.50457296725822687, 15.20507249208304046 ) ) ;
#3574 = COLOUR_RGB ( '', 0.72549020, 0.75294118, 0.79215686) ;
#3575 = DIRECTION ( 'NONE',  ( 0.000000000000000000, 0.000000000000000000, -1.000000000000000000 ) ) ;
#3576 = SHAPE_REPRESENTATION ( 'Stainless Steel Outer Casing', ( #1791 ), #15487 ) ;
#3577 = CARTESIAN_POINT ( 'NONE',  ( -19.95583473709191580, -22.49542703274176603, 18.91992750791694888 ) ) ;
#3578 = FACE_OUTER_BOUND ( 'NONE', #11546, .T. ) ;
#3579 = CARTESIAN_POINT ( 'NONE',  ( -16.50457296725820555, -28.95583473709189803, 28.10742750791695954 ) ) ;
#3580 = CARTESIAN_POINT ( 'NONE',  ( 0.000000000000000000, 64.00000000000000000, 49.99999999999999289 ) ) ;
#3581 = CARTESIAN_POINT ( 'NONE',  ( -19.41254052147350961, -21.64274437364857562, 21.11132249208304401 ) ) ;
#3582 = CARTESIAN_POINT ( 'NONE',  ( -0.8561741729129465073, 61.93301270000000613, 49.10000000109246088 ) ) ;
#3583 = DIRECTION ( 'NONE',  ( 0.000000000000000000, 1.000000000000000000, 0.000000000000000000 ) ) ;
#3584 = DIRECTION ( 'NONE',  ( -1.000000000000000000, 0.000000000000000000, 0.000000000000000000 ) ) ;
#3585 =( NAMED_UNIT ( * ) SI_UNIT ( $, .STERADIAN. ) SOLID_ANGLE_UNIT ( ) );
#3586 = CARTESIAN_POINT ( 'NONE',  ( 1.461580736456473906, 62.53841926354353120, 49.25000000109246656 ) ) ;
#3587 = CARTESIAN_POINT ( 'NONE',  ( -24.00000000000000000, 53.00000000000000711, -12.49999999999999645 ) ) ;
#3588 = PRESENTATION_LAYER_ASSIGNMENT (  '', '', ( #17058 ) ) ;
#3589 = VECTOR ( 'NONE', #12199, 1000.000000000000000 ) ;
#3590 = VERTEX_POINT ( 'NONE', #7779 ) ;
#3591 = CARTESIAN_POINT ( 'NONE',  ( -20.24501739517669563, -18.99630608921239627, 37.08007249208304046 ) ) ;
#3592 = CARTESIAN_POINT ( 'NONE',  ( -20.04416526290809131, -22.82508104294700502, 10.39257249208303868 ) ) ;
#3593 = CARTESIAN_POINT ( 'NONE',  ( -15.16482700510260706, -26.99999999999998579, 33.13867750791695954 ) ) ;
#3594 = LINE ( 'NONE', #14182, #8318 ) ;
#3595 = CARTESIAN_POINT ( 'NONE',  ( -11.64274437364859693, -17.85540867095757989, 22.42382249208304046 ) ) ;
#3596 = CARTESIAN_POINT ( 'NONE',  ( 3.796994071234847710E-16, 61.93301269999999903, 46.55000000109247082 ) ) ;
#3597 = CARTESIAN_POINT ( 'NONE',  ( 3.796994071234847710E-16, 61.93301269999999903, 44.95000000109246940 ) ) ;
#3598 = ORIENTED_EDGE ( 'NONE', *, *, #3600, .T. ) ;
#3599 = ORIENTED_EDGE ( 'NONE', *, *, #13350, .T. ) ;
#3600 = EDGE_CURVE ( 'NONE', #13252, #2050, #16998, .T. ) ;
#3601 =( GEOMETRIC_REPRESENTATION_CONTEXT ( 3 ) GLOBAL_UNCERTAINTY_ASSIGNED_CONTEXT ( ( #1601 ) ) GLOBAL_UNIT_ASSIGNED_CONTEXT ( ( #14848, #1123, #5737 ) ) REPRESENTATION_CONTEXT ( 'NONE', 'WORKASPACE' ) );
#3602 = CARTESIAN_POINT ( 'NONE',  ( -31.74999999999995737, 0.000000000000000000, 0.000000000000000000 ) ) ;
#3603 = CARTESIAN_POINT ( 'NONE',  ( -41.00000000000000711, 110.0000000000000000, 21.00000000000000355 ) ) ;
#3604 = CIRCLE ( 'NONE', #14551, 1.249999999999999334 ) ;
#3605 = CARTESIAN_POINT ( 'NONE',  ( -1.461580736456473906, 65.46158073645646880, 49.45000000109246940 ) ) ;
#3606 = CARTESIAN_POINT ( 'NONE',  ( -32.50000000000001421, -6.000000000000000000, 42.49999999999997868 ) ) ;
#3607 = EDGE_CURVE ( 'NONE', #19340, #17432, #18467, .T. ) ;
#3608 = CARTESIAN_POINT ( 'NONE',  ( -40.00000000000000711, 53.00000000000000711, -24.49999999999999645 ) ) ;
#3609 = DIRECTION ( 'NONE',  ( -1.000000000000000000, 0.000000000000000000, -0.000000000000000000 ) ) ;
#3610 = ADVANCED_FACE ( 'NONE', ( #12375 ), #13850, .T. ) ;
#3611 = MANIFOLD_SOLID_BREP ( 'Hex', #17932 ) ;
#3612 = CARTESIAN_POINT ( 'NONE',  ( 0.2500000000000002220, 0.000000000000000000, 4.000000000000000000 ) ) ;
#3613 = VERTEX_POINT ( 'NONE', #15518 ) ;
#3614 = VERTEX_POINT ( 'NONE', #16894 ) ;
#3615 = CARTESIAN_POINT ( 'NONE',  ( -22.04416526290807710, -25.71081734191525925, 34.23242750791695244 ) ) ;
#3616 = CARTESIAN_POINT ( 'NONE',  ( -14.99999999999999645, 52.00000000000000711, 26.99999999999997868 ) ) ;
#3617 = ORIENTED_EDGE ( 'NONE', *, *, #7860, .F. ) ;
#3618 = AXIS2_PLACEMENT_3D ( 'NONE', #11931, #17924, #2128 ) ;
#3620 = ORIENTED_EDGE ( 'NONE', *, *, #9152, .T. ) ;
#3619 = VERTEX_POINT ( 'NONE', #1898 ) ;
#3621 = CARTESIAN_POINT ( 'NONE',  ( -14.36097942780925685, -20.95583473709189093, 37.95507249208304046 ) ) ;
#3622 = CARTESIAN_POINT ( 'NONE',  ( -22.04416526290807710, -25.71081734191525925, 23.73242750791695954 ) ) ;
#3623 = CARTESIAN_POINT ( 'NONE',  ( -14.99999999999999645, 73.00000000000001421, 20.99999999999998224 ) ) ;
#3624 = CARTESIAN_POINT ( 'NONE',  ( -1.035533905932738641, 66.50000000000000000, 49.15000000218494591 ) ) ;
#3625 = DIRECTION ( 'NONE',  ( 1.000000000000000000, 1.734723475976807094E-15, -0.000000000000000000 ) ) ;
#3626 = ORIENTED_EDGE ( 'NONE', *, *, #18436, .T. ) ;
#3627 = CARTESIAN_POINT ( 'NONE',  ( -17.95583473709191580, -23.03132541760400898, 24.16992750791696309 ) ) ;
#3628 = EDGE_CURVE ( 'NONE', #15935, #12535, #7883, .T. ) ;
#3629 = LINE ( 'NONE', #15401, #8186 ) ;
#3630 = VERTEX_POINT ( 'NONE', #9435 ) ;
#3631 = DIRECTION ( 'NONE',  ( 0.000000000000000000, 0.7071067811865490160, -0.7071067811865461294 ) ) ;
#3632 = VERTEX_POINT ( 'NONE', #15428 ) ;
#3633 = CARTESIAN_POINT ( 'NONE',  ( -50.00000000000002132, 16.75735931288065572, 56.99999999999997158 ) ) ;
#3634 = FACE_BOUND ( 'NONE', #5753, .T. ) ;
#3635 = CARTESIAN_POINT ( 'NONE',  ( 3.399999999999996803, 29.47747564417430155, 56.65425233947098604 ) ) ;
#3636 = VECTOR ( 'NONE', #12113, 1000.000000000000227 ) ;
#3637 = CARTESIAN_POINT ( 'NONE',  ( -2.066987300000001859, 64.85617417291294373, 48.70000000109247651 ) ) ;
#3638 = VECTOR ( 'NONE', #15142, 1000.000000000000000 ) ;
#3639 = CARTESIAN_POINT ( 'NONE',  ( -1.461580736456473906, 65.46158073645646880, 47.25000000109246656 ) ) ;
#3640 = CARTESIAN_POINT ( 'NONE',  ( 2.500000000000000000, 0.000000000000000000, 0.000000000000000000 ) ) ;
#3641 = CARTESIAN_POINT ( 'NONE',  ( -19.99999999999999645, -52.00000000000000711, 1.500000000000000000 ) ) ;
#3642 = CARTESIAN_POINT ( 'NONE',  ( -1.530808498934192803E-16, 66.50000000000000000, 45.00000000000000000 ) ) ;
#3643 = EDGE_LOOP ( 'NONE', ( #7791, #3319, #1304, #15009 ) ) ;
#3644 = CARTESIAN_POINT ( 'NONE',  ( -14.83517299489739649, -18.99999999999997868, 35.76367750791695954 ) ) ;
#3645 = CARTESIAN_POINT ( 'NONE',  ( -41.00000000000000711, 53.00000000000000711, -6.000000000000001776 ) ) ;
#3646 = EDGE_CURVE ( 'NONE', #4945, #17638, #12573, .T. ) ;
#3647 = EDGE_LOOP ( 'NONE', ( #17612, #18444, #16454 ) ) ;
#3648 = ADVANCED_FACE ( 'NONE', ( #1992 ), #9238, .F. ) ;
#3649 = CARTESIAN_POINT ( 'NONE',  ( -9.999999999999994671, -23.83517299489734143, 28.54882249208304401 ) ) ;
#3650 = EDGE_CURVE ( 'NONE', #4220, #4614, #13944, .T. ) ;
#3651 = AXIS2_PLACEMENT_3D ( 'NONE', #7370, #16394, #4540 ) ;
#3652 = VECTOR ( 'NONE', #7075, 1000.000000000000000 ) ;
#3653 = CARTESIAN_POINT ( 'NONE',  ( -16.64274437364858272, -21.48433729119797420, 32.04882249208304756 ) ) ;
#3654 =( LENGTH_UNIT ( ) NAMED_UNIT ( * ) SI_UNIT ( .MILLI., .METRE. ) );
#3655 = ORIENTED_EDGE ( 'NONE', *, *, #5788, .T. ) ;
#3656 = DIRECTION ( 'NONE',  ( 0.000000000000000000, 0.000000000000000000, 1.000000000000000000 ) ) ;
#3657 = ORIENTED_EDGE ( 'NONE', *, *, #10824, .F. ) ;
#3658 = CARTESIAN_POINT ( 'NONE',  ( -1.530808498934192803E-16, 66.50000000000000000, 45.10000000218494165 ) ) ;
#3659 = DIRECTION ( 'NONE',  ( -1.000000000000000000, -0.000000000000000000, -0.000000000000000000 ) ) ;
#3660 = DIRECTION ( 'NONE',  ( -1.000000000000000000, -0.000000000000000000, -0.000000000000000000 ) ) ;
#3661 = VECTOR ( 'NONE', #1983, 1000.000000000000000 ) ;
#3662 = ADVANCED_FACE ( 'NONE', ( #15229 ), #6695, .F. ) ;
#3663 = PLANE ( 'NONE',  #8574 ) ;
#3664 = EDGE_CURVE ( 'NONE', #3619, #15191, #12661, .T. ) ;
#3665 = CYLINDRICAL_SURFACE ( 'NONE', #5671, 1.599999999999997202 ) ;
#3666 = LINE ( 'NONE', #6616, #3950 ) ;
#3667 = LINE ( 'NONE', #4583, #12398 ) ;
#3668 = ORIENTED_EDGE ( 'NONE', *, *, #13567, .T. ) ;
#3669 = CARTESIAN_POINT ( 'NONE',  ( -17.64274437364855430, -28.24771351637087236, 33.57617750791696665 ) ) ;
#3670 = CARTESIAN_POINT ( 'NONE',  ( -2.500000000000001776, 64.00000000000000000, 44.50000000218494733 ) ) ;
#3671 = CARTESIAN_POINT ( 'NONE',  ( -18.53959229564982536, -27.78091578003890660, 35.76757249208302625 ) ) ;
#3672 = MECHANICAL_DESIGN_GEOMETRIC_PRESENTATION_REPRESENTATION (  '', ( #5247 ), #6190 ) ;
#3673 = FACE_OUTER_BOUND ( 'NONE', #17092, .T. ) ;
#3674 = CARTESIAN_POINT ( 'NONE',  ( -17.35725562635144215, -19.58745947852648683, 14.32617750791695777 ) ) ;
#3675 = DIRECTION ( 'NONE',  ( 0.000000000000000000, -0.000000000000000000, 1.000000000000000000 ) ) ;
#3676 = CARTESIAN_POINT ( 'NONE',  ( -11.21908421996108984, -20.46040770435011069, 31.16992750791695599 ) ) ;
#3677 = DIRECTION ( 'NONE',  ( -0.000000000000000000, -1.000000000000000000, -0.000000000000000000 ) ) ;
#3678 = CARTESIAN_POINT ( 'NONE',  ( -9.999999999999994671, -23.83517299489734143, 28.54882249208304401 ) ) ;
#3679 = CARTESIAN_POINT ( 'NONE',  ( 1.767766952966369987, 65.76776695296638309, 49.69999999999999574 ) ) ;
#3680 = FACE_OUTER_BOUND ( 'NONE', #8622, .T. ) ;
#3681 = CARTESIAN_POINT ( 'NONE',  ( -40.00000000000000711, 113.0000000000000000, -32.00000000000000000 ) ) ;
#3682 = EDGE_CURVE ( 'NONE', #14586, #17642, #11183, .T. ) ;
#3683 = DIRECTION ( 'NONE',  ( 0.000000000000000000, 0.000000000000000000, -1.000000000000000000 ) ) ;
#3684 = CARTESIAN_POINT ( 'NONE',  ( 0.8561741729129472844, 61.93301270000000613, 47.60000000109246798 ) ) ;
#3685 = DIRECTION ( 'NONE',  ( -1.000000000000000000, 0.000000000000000000, 0.000000000000000000 ) ) ;
#3686 = VERTEX_POINT ( 'NONE', #8352 ) ;
#3687 = CARTESIAN_POINT ( 'NONE',  ( -13.28918265808478694, -16.95583473709189093, 37.95507249208304046 ) ) ;
#3688 = CARTESIAN_POINT ( 'NONE',  ( -0.8561741729129461742, 66.06698730000000808, 46.20000000109248361 ) ) ;
#3689 = CARTESIAN_POINT ( 'NONE',  ( -18.04416526290808420, -24.63902057219074493, 23.73242750791696665 ) ) ;
#3690 = APPLICATION_CONTEXT ( 'automotive_design' ) ;
#3691 = DIRECTION ( 'NONE',  ( 4.081702296416016490E-16, -0.000000000000000000, 1.000000000000000000 ) ) ;
#3692 = CARTESIAN_POINT ( 'NONE',  ( -7.955834737091903364, -25.71081734191518464, 23.51757249208304401 ) ) ;
#3693 = CARTESIAN_POINT ( 'NONE',  ( -2.066987300000001415, 63.14382582708705627, 46.40000000109246514 ) ) ;
#3694 = ORIENTED_EDGE ( 'NONE', *, *, #14060, .F. ) ;
#3695 = VERTEX_POINT ( 'NONE', #9807 ) ;
#3696 = CARTESIAN_POINT ( 'NONE',  ( 2.500000000000000000, -1.768423874527825124, -1.020999999999998575 ) ) ;
#3697 = CARTESIAN_POINT ( 'NONE',  ( -40.00000000000000000, 53.00000000000000711, -6.000000000000001776 ) ) ;
#3698 = CARTESIAN_POINT ( 'NONE',  ( -2.066987300000001415, 64.85617417291294373, 45.50000000109247367 ) ) ;
#3699 = DIRECTION ( 'NONE',  ( -0.000000000000000000, -0.7071067811865456854, -0.7071067811865493491 ) ) ;
#3700 = DIRECTION ( 'NONE',  ( 1.000000000000000000, 0.000000000000000000, 0.000000000000000000 ) ) ;
#3701 = ADVANCED_FACE ( 'NONE', ( #6788 ), #992, .F. ) ;
#3702 = CARTESIAN_POINT ( 'NONE',  ( -7.999999999999986677, 68.00000000000000000, 66.99999999999997158 ) ) ;
#3703 = CARTESIAN_POINT ( 'NONE',  ( -24.00000000000000000, 52.00000000000000711, 30.00000000000000000 ) ) ;
#3704 = VERTEX_POINT ( 'NONE', #11558 ) ;
#3705 = ORIENTED_EDGE ( 'NONE', *, *, #10956, .T. ) ;
#3706 = CARTESIAN_POINT ( 'NONE',  ( -20.00369391078762860, -18.75498260482333279, 29.85742750791695599 ) ) ;
#3707 =( LENGTH_UNIT ( ) NAMED_UNIT ( * ) SI_UNIT ( .MILLI., .METRE. ) );
#3708 = ORIENTED_EDGE ( 'NONE', *, *, #13973, .F. ) ;
#3710 = VERTEX_POINT ( 'NONE', #10088 ) ;
#3709 = ORIENTED_EDGE ( 'NONE', *, *, #13504, .T. ) ;
#3711 = CARTESIAN_POINT ( 'NONE',  ( -13.64274437364857739, -21.31951028609534760, 32.92382249208304046 ) ) ;
#3712 = CARTESIAN_POINT ( 'NONE',  ( -8.044165262908075320, -26.04047135212042718, 16.29492750791696309 ) ) ;
#3713 = AXIS2_PLACEMENT_3D ( 'NONE', #18895, #17322, #1041 ) ;
#3714 = PLANE ( 'NONE',  #9451 ) ;
#3715 = CARTESIAN_POINT ( 'NONE',  ( 2.500000000000001776, 64.00000000000000000, 48.90000000218494591 ) ) ;
#3716 = CARTESIAN_POINT ( 'NONE',  ( -40.00000000000000711, 110.0000000000000000, 0.5000000000000004441 ) ) ;
#3717 = VERTEX_POINT ( 'NONE', #9901 ) ;
#3718 = CARTESIAN_POINT ( 'NONE',  ( -12.04416526290807887, -24.96867458239596260, 32.04492750791695954 ) ) ;
#3719 = DIRECTION ( 'NONE',  ( 1.000000000000000000, -0.000000000000000000, 0.000000000000000000 ) ) ;
#3720 = ORIENTED_EDGE ( 'NONE', *, *, #15157, .T. ) ;
#3721 = CARTESIAN_POINT ( 'NONE',  ( -24.00000000000000000, 53.00000000000000711, 30.00000000000000000 ) ) ;
#3722 = VERTEX_POINT ( 'NONE', #800 ) ;
#3723 = CARTESIAN_POINT ( 'NONE',  ( 0.5387381024323600887, 61.98586169951557423, 44.99999999999999289 ) ) ;
#3724 = DIRECTION ( 'NONE',  ( 0.000000000000000000, 0.000000000000000000, 1.000000000000000000 ) ) ;
#3725 = LINE ( 'NONE', #10883, #17836 ) ;
#3726 = AXIS2_PLACEMENT_3D ( 'NONE', #7114, #5943, #65 ) ;
#3727 = CARTESIAN_POINT ( 'NONE',  ( -1.461580736456473462, 62.53841926354353120, 47.25000000109247367 ) ) ;
#3728 = CARTESIAN_POINT ( 'NONE',  ( -1.265664690411616068E-16, 66.06698730000000808, 48.75000000109246656 ) ) ;
#3729 = CARTESIAN_POINT ( 'NONE',  ( -4.999999999999980460, 60.00000000000000711, 69.99999999999998579 ) ) ;
#3730 = VECTOR ( 'NONE', #3486, 1000.000000000000000 ) ;
#3731 = FACE_OUTER_BOUND ( 'NONE', #13883, .T. ) ;
#3732 = FACE_OUTER_BOUND ( 'NONE', #12990, .T. ) ;
#3733 = ORIENTED_EDGE ( 'NONE', *, *, #2687, .T. ) ;
#3734 = ORIENTED_EDGE ( 'NONE', *, *, #11216, .T. ) ;
#3735 = ADVANCED_FACE ( 'NONE', ( #14417 ), #2278, .T. ) ;
#3737 = EDGE_CURVE ( 'NONE', #7027, #16441, #12251, .T. ) ;
#3736 = CARTESIAN_POINT ( 'NONE',  ( -19.41254052147348830, -26.35725562635142083, 34.01367750791696665 ) ) ;
#3738 = CARTESIAN_POINT ( 'NONE',  ( -41.00000000000000711, 53.00000000000000711, -32.00000000000000000 ) ) ;
#3739 = ORIENTED_EDGE ( 'NONE', *, *, #6928, .T. ) ;
#3740 = CARTESIAN_POINT ( 'NONE',  ( -19.95583473709190514, -25.50457296725822687, 30.95507249208303691 ) ) ;
#3741 = MANIFOLD_SOLID_BREP ( 'Boss-Extrude5', #1016 ) ;
#3742 = AXIS2_PLACEMENT_3D ( 'NONE', #3466, #5040, #15432 ) ;
#3743 = DIRECTION ( 'NONE',  ( -0.000000000000000000, 1.320393690296331133E-15, 1.000000000000000000 ) ) ;
#3744 = CARTESIAN_POINT ( 'NONE',  ( -17.99999999999999645, -24.16482700510260173, 25.92382249208304756 ) ) ;
#3745 = AXIS2_PLACEMENT_3D ( 'NONE', #4252, #17774, #2769 ) ;
#3746 = FILL_AREA_STYLE ('',( #2368 ) ) ;
#3747 = ORIENTED_EDGE ( 'NONE', *, *, #12665, .T. ) ;
#3748 = VECTOR ( 'NONE', #10264, 1000.000000000000000 ) ;
#3749 = CARTESIAN_POINT ( 'NONE',  ( -41.00000000000000711, 53.00000000000000711, -45.00000000000000000 ) ) ;
#3750 = EDGE_LOOP ( 'NONE', ( #9954, #17956, #8330, #10933 ) ) ;
#3751 = DIRECTION ( 'NONE',  ( 0.000000000000000000, 0.000000000000000000, 1.000000000000000000 ) ) ;
#3752 = LINE ( 'NONE', #5041, #10802 ) ;
#3753 = CARTESIAN_POINT ( 'NONE',  ( 37.50000000000000711, -6.000000000000000000, -45.00000000000000000 ) ) ;
#3754 = EDGE_CURVE ( 'NONE', #2028, #10481, #5702, .T. ) ;
#3755 = EDGE_CURVE ( 'NONE', #1836, #292, #18844, .T. ) ;
#3756 = VECTOR ( 'NONE', #3751, 1000.000000000000000 ) ;
#3757 = DIRECTION ( 'NONE',  ( 0.000000000000000000, -0.000000000000000000, 1.000000000000000000 ) ) ;
#3758 = DIRECTION ( 'NONE',  ( 0.000000000000000000, 0.000000000000000000, 1.000000000000000000 ) ) ;
#3759 = LINE ( 'NONE', #15725, #3005 ) ;
#3760 = AXIS2_PLACEMENT_3D ( 'NONE', #16578, #16482, #10485 ) ;
#3761 = DIRECTION ( 'NONE',  ( 1.000000000000000000, 0.000000000000000000, 0.000000000000000000 ) ) ;
#3762 = UNCERTAINTY_MEASURE_WITH_UNIT (LENGTH_MEASURE( 1.000000000000000082E-05 ), #3707, 'distance_accuracy_value', 'NONE');
#3763 = ORIENTED_EDGE ( 'NONE', *, *, #9077, .F. ) ;
#3764 = CARTESIAN_POINT ( 'NONE',  ( -13.49542703274178379, -19.04416526290806289, 25.48242750791694888 ) ) ;
#3765 = VECTOR ( 'NONE', #15296, 1000.000000000000114 ) ;
#3766 = CARTESIAN_POINT ( 'NONE',  ( -2.066987300000001859, 64.85617417291294373, 47.10000000109246798 ) ) ;
#3767 = CARTESIAN_POINT ( 'NONE',  ( -15.16482700510263371, -18.99999999999997868, 37.73632249208303335 ) ) ;
#3768 = AXIS2_PLACEMENT_3D ( 'NONE', #19053, #10214, #5727 ) ;
#3769 = CARTESIAN_POINT ( 'NONE',  ( 44.99999999999997158, 3.000000000000000000, 56.50000000000000000 ) ) ;
#3770 = CARTESIAN_POINT ( 'NONE',  ( -9.999999999999994671, -24.16482700510257686, 26.57617750791695954 ) ) ;
#3771 = CARTESIAN_POINT ( 'NONE',  ( -41.00000000000000711, 53.00000000000000711, 14.50000000000000000 ) ) ;
#3772 = CARTESIAN_POINT ( 'NONE',  ( -18.53959229564986799, -20.21908421996107563, 29.85742750791695599 ) ) ;
#3773 = VECTOR ( 'NONE', #14128, 1000.000000000000000 ) ;
#3774 = CARTESIAN_POINT ( 'NONE',  ( 1.767766952966369987, 65.76776695296638309, 46.60000000218494165 ) ) ;
#3775 = CARTESIAN_POINT ( 'NONE',  ( -13.82508104294702100, -18.95583473709188382, 22.20507249208304401 ) ) ;
#3776 = EDGE_CURVE ( 'NONE', #15097, #4424, #9989, .T. ) ;
#3777 = ADVANCED_FACE ( 'NONE', ( #11367 ), #17275, .T. ) ;
#3778 = CARTESIAN_POINT ( 'NONE',  ( -1.530808498934192803E-16, 66.50000000000000000, 48.99999999999999289 ) ) ;
#3779 = LINE ( 'NONE', #18773, #1198 ) ;
#3780 = VECTOR ( 'NONE', #17971, 1000.000000000000000 ) ;
#3781 = CARTESIAN_POINT ( 'NONE',  ( 2.500000000000001776, 64.00000000000000000, 48.90000000218494591 ) ) ;
#3782 = ADVANCED_FACE ( 'NONE', ( #15710 ), #8628, .F. ) ;
#3783 = CARTESIAN_POINT ( 'NONE',  ( -0.8561741729129461742, 66.06698729999999387, 44.80000000109246372 ) ) ;
#3784 = LINE ( 'NONE', #11315, #5515 ) ;
#3785 = VECTOR ( 'NONE', #11964, 1000.000000000000000 ) ;
#3786 = ORIENTED_EDGE ( 'NONE', *, *, #6175, .F. ) ;
#3787 = VECTOR ( 'NONE', #14568, 1000.000000000000000 ) ;
#3788 = SURFACE_SIDE_STYLE ('',( #18696 ) ) ;
#3789 = CARTESIAN_POINT ( 'NONE',  ( -2.066987300000000971, 63.14382582708704916, 46.40000000109247225 ) ) ;
#3790 = CARTESIAN_POINT ( 'NONE',  ( -13.64274437364856141, -26.68048971390460622, 27.45117750791696309 ) ) ;
#3791 = CYLINDRICAL_SURFACE ( 'NONE', #18227, 2.500000000000002220 ) ;
#3792 = CARTESIAN_POINT ( 'NONE',  ( -7.999999999999996447, -23.83517299489733432, 39.04882249208302625 ) ) ;
#3793 = AXIS2_PLACEMENT_3D ( 'NONE', #2456, #8442, #3841 ) ;
#3794 = CARTESIAN_POINT ( 'NONE',  ( 1.461580736456473906, 62.53841926354353120, 45.85000000109246798 ) ) ;
#3795 = EDGE_CURVE ( 'NONE', #16140, #996, #19224, .T. ) ;
#3796 = VERTEX_POINT ( 'NONE', #1485 ) ;
#3797 = DIRECTION ( 'NONE',  ( -0.000000000000000000, -0.000000000000000000, -1.000000000000000000 ) ) ;
#3798 = DIRECTION ( 'NONE',  ( 2.775557561562890858E-16, 0.7071067811865454633, 0.7071067811865496822 ) ) ;
#3799 = VECTOR ( 'NONE', #6794, 1000.000000000000000 ) ;
#3800 = CARTESIAN_POINT ( 'NONE',  ( 2.066987300000001415, 64.00000000000000000, 45.15000000109247225 ) ) ;
#3801 = CARTESIAN_POINT ( 'NONE',  ( 7.500000000000005329, -38.00000000000000000, 9.500000000000001776 ) ) ;
#3802 = CARTESIAN_POINT ( 'NONE',  ( -2.500000000000001776, 64.00000000000000000, 49.30000000218494449 ) ) ;
#3803 = CARTESIAN_POINT ( 'NONE',  ( 4.592425496802577917E-16, 61.50000000000000000, 48.59999999999999432 ) ) ;
#3804 = CARTESIAN_POINT ( 'NONE',  ( -41.99999999999997868, 139.6861997365471950, -52.00000000000000000 ) ) ;
#3805 = ORIENTED_EDGE ( 'NONE', *, *, #1500, .F. ) ;
#3806 = ORIENTED_EDGE ( 'NONE', *, *, #4837, .T. ) ;
#3807 = CARTESIAN_POINT ( 'NONE',  ( -15.16482700510258574, -30.99999999999998224, 27.88867750791695954 ) ) ;
#3808 = FILL_AREA_STYLE_COLOUR ( '', #10541 ) ;
#3809 = ORIENTED_EDGE ( 'NONE', *, *, #15473, .T. ) ;
#3811 = EDGE_LOOP ( 'NONE', ( #4293, #15845, #8985, #10486, #15467, #15193 ) ) ;
#3810 = ORIENTED_EDGE ( 'NONE', *, *, #9670, .F. ) ;
#3812 = CARTESIAN_POINT ( 'NONE',  ( -15.96867458239599635, -21.04416526290806999, 27.01757249208303691 ) ) ;
#3813 = CARTESIAN_POINT ( 'NONE',  ( -22.04416526290807710, -25.71081734191525925, 28.98242750791695599 ) ) ;
#3814 = VECTOR ( 'NONE', #17152, 1000.000000000000000 ) ;
#3815 = CARTESIAN_POINT ( 'NONE',  ( -2.500000000000001776, 64.00000000000000000, 47.59999999999999432 ) ) ;
#3816 = CARTESIAN_POINT ( 'NONE',  ( -1.035533905932738863, 61.50000000000000000, 46.25000000218494733 ) ) ;
#3817 = DIRECTION ( 'NONE',  ( 0.000000000000000000, 0.000000000000000000, 1.000000000000000000 ) ) ;
#3818 = ORIENTED_EDGE ( 'NONE', *, *, #7861, .F. ) ;
#3819 = DIRECTION ( 'NONE',  ( -0.000000000000000000, 0.7071067811865456854, 0.7071067811865493491 ) ) ;
#3820 = ORIENTED_EDGE ( 'NONE', *, *, #18436, .F. ) ;
#3821 = DIRECTION ( 'NONE',  ( 0.000000000000000000, 0.000000000000000000, 1.000000000000000000 ) ) ;
#3822 = ORIENTED_EDGE ( 'NONE', *, *, #18, .F. ) ;
#3823 = CARTESIAN_POINT ( 'NONE',  ( -1.366300952416055425, 62.44303698707672368, 45.00000000000000711 ) ) ;
#3824 = PLANE ( 'NONE',  #4039 ) ;
#3825 = DIRECTION ( 'NONE',  ( 3.491481338843133355E-15, 0.7071067811865495711, -0.7071067811865454633 ) ) ;
#3826 = CARTESIAN_POINT ( 'NONE',  ( -0.8561741729129461742, 66.06698729999999387, 44.60000000109246088 ) ) ;
#3827 = CARTESIAN_POINT ( 'NONE',  ( -0.8561741729129461742, 66.06698730000000808, 49.60000000109247509 ) ) ;
#3828 = FACE_OUTER_BOUND ( 'NONE', #197, .T. ) ;
#3829 = CIRCLE ( 'NONE', #14785, 1.500000000000001332 ) ;
#3830 = CARTESIAN_POINT ( 'NONE',  ( 7.500000000000005329, -26.00000000000000000, 9.500000000000001776 ) ) ;
#3831 = FACE_OUTER_BOUND ( 'NONE', #10868, .T. ) ;
#3832 = EDGE_LOOP ( 'NONE', ( #11545, #18861, #5494, #11294 ) ) ;
#3833 = ORIENTED_EDGE ( 'NONE', *, *, #8201, .F. ) ;
#3834 = CARTESIAN_POINT ( 'NONE',  ( -14.83517299489739649, -18.99999999999997868, 30.51367750791695954 ) ) ;
#3835 = CARTESIAN_POINT ( 'NONE',  ( -24.00000000000000000, 110.0000000000000000, 30.00000000000000000 ) ) ;
#3836 = ORIENTED_EDGE ( 'NONE', *, *, #4490, .T. ) ;
#3837 = VECTOR ( 'NONE', #16551, 1000.000000000000000 ) ;
#3838 = CARTESIAN_POINT ( 'NONE',  ( -19.41254052147350961, -21.64274437364857562, 31.61132249208303691 ) ) ;
#3839 = DIRECTION ( 'NONE',  ( 0.000000000000000000, -0.7071067811865495711, 0.7071067811865454633 ) ) ;
#3840 = CARTESIAN_POINT ( 'NONE',  ( -17.99999999999999645, -24.16482700510260173, 31.17382249208304046 ) ) ;
#3841 = DIRECTION ( 'NONE',  ( -1.000000000000000000, 0.000000000000000000, -0.000000000000000000 ) ) ;
#3842 = VERTEX_POINT ( 'NONE', #5793 ) ;
#3843 = DIRECTION ( 'NONE',  ( 0.000000000000000000, 0.000000000000000000, 1.000000000000000000 ) ) ;
#3844 = ORIENTED_EDGE ( 'NONE', *, *, #13213, .T. ) ;
#3845 = DIRECTION ( 'NONE',  ( -1.000000000000000000, 0.000000000000000000, 0.000000000000000000 ) ) ;
#3846 = EDGE_CURVE ( 'NONE', #6167, #8073, #2747, .T. ) ;
#3847 = EDGE_CURVE ( 'NONE', #7381, #12041, #17754, .T. ) ;
#3848 = CARTESIAN_POINT ( 'NONE',  ( -32.50000000000000000, 52.00000000000000711, 17.49999999999999645 ) ) ;
#3849 = DIRECTION ( 'NONE',  ( 0.000000000000000000, 0.000000000000000000, 1.000000000000000000 ) ) ;
#3850 = EDGE_CURVE ( 'NONE', #7747, #13196, #3045, .T. ) ;
#3851 = FACE_BOUND ( 'NONE', #7440, .T. ) ;
#3852 = PLANE ( 'NONE',  #3185 ) ;
#3854 = ADVANCED_FACE ( 'NONE', ( #13423 ), #5995, .T. ) ;
#3853 = DIRECTION ( 'NONE',  ( 0.000000000000000000, 0.000000000000000000, -1.000000000000000000 ) ) ;
#3855 = DIRECTION ( 'NONE',  ( -0.5773502691896255090, 0.8164965809277261455, 0.000000000000000000 ) ) ;
#3856 = ORIENTED_EDGE ( 'NONE', *, *, #8335, .F. ) ;
#3857 = VERTEX_POINT ( 'NONE', #13531 ) ;
#3858 = CARTESIAN_POINT ( 'NONE',  ( -11.46040770435012668, -27.78091578003887463, 27.23242750791694888 ) ) ;
#3859 = CARTESIAN_POINT ( 'NONE',  ( -0.8561741729129465073, 61.93301270000000613, 48.90000000109247225 ) ) ;
#3860 = CARTESIAN_POINT ( 'NONE',  ( -12.35725562635140307, -28.24771351637085459, 39.92382249208304046 ) ) ;
#3861 = FACE_BOUND ( 'NONE', #1383, .T. ) ;
#3862 = CARTESIAN_POINT ( 'NONE',  ( -17.64274437364855430, -28.24771351637087236, 33.57617750791696665 ) ) ;
#3863 = CARTESIAN_POINT ( 'NONE',  ( -41.00000000000000711, 53.00000000000000711, -19.00000000000000000 ) ) ;
#3864 = CARTESIAN_POINT ( 'NONE',  ( -10.58745947852649927, -21.64274437364853654, 31.38867750791696309 ) ) ;
#3865 = CARTESIAN_POINT ( 'NONE',  ( 4.189607678530260948, 26.72836399182260791, 59.40336399182267257 ) ) ;
#3866 = CARTESIAN_POINT ( 'NONE',  ( -19.95583473709190514, -25.50457296725823042, 20.45507249208304046 ) ) ;
#3867 = CARTESIAN_POINT ( 'NONE',  ( -1.035533905932738863, 61.50000000000000000, 49.35000000000000142 ) ) ;
#3868 = CARTESIAN_POINT ( 'NONE',  ( 3.796994071234847710E-16, 61.93301269999999903, 49.15000000109246514 ) ) ;
#3869 = CARTESIAN_POINT ( 'NONE',  ( 4.592425496802577917E-16, 61.50000000000000000, 48.70000000218494307 ) ) ;
#3870 = CARTESIAN_POINT ( 'NONE',  ( -1.265664690411616068E-16, 66.06698730000000808, 45.55000000109246372 ) ) ;
#3871 = DIRECTION ( 'NONE',  ( 1.000000000000000000, -0.000000000000000000, -0.000000000000000000 ) ) ;
#3872 = ORIENTED_EDGE ( 'NONE', *, *, #1500, .T. ) ;
#3873 = EDGE_CURVE ( 'NONE', #4404, #17838, #6091, .T. ) ;
#3874 = CARTESIAN_POINT ( 'NONE',  ( 1.844224359752661968, -38.39960408384397539, 1.500000000000000000 ) ) ;
#3875 = EDGE_CURVE ( 'NONE', #17639, #16538, #13617, .T. ) ;
#3876 = CARTESIAN_POINT ( 'NONE',  ( -17.64274437364855430, -28.24771351637087236, 2.076177507916958209 ) ) ;
#3877 = DIRECTION ( 'NONE',  ( -0.000000000000000000, 1.000000000000000000, -0.000000000000000000 ) ) ;
#3878 = EDGE_CURVE ( 'NONE', #12574, #7648, #9420, .T. ) ;
#3879 = CARTESIAN_POINT ( 'NONE',  ( -20.24501739517669563, -18.99630608921239627, 31.83007249208304046 ) ) ;
#3880 = CARTESIAN_POINT ( 'NONE',  ( -0.8561741729129461742, 66.06698729999999387, 48.00000000109246656 ) ) ;
#3881 = VERTEX_POINT ( 'NONE', #16576 ) ;
#3882 = EDGE_CURVE ( 'NONE', #12628, #17940, #15109, .T. ) ;
#3883 = LINE ( 'NONE', #18704, #19103 ) ;
#3884 = LINE ( 'NONE', #14467, #9743 ) ;
#3885 = CARTESIAN_POINT ( 'NONE',  ( 1.300000000000000044, -0.7390083445627200209, 1.280000000000001137 ) ) ;
#3886 = LINE ( 'NONE', #6827, #2150 ) ;
#3887 = CARTESIAN_POINT ( 'NONE',  ( -50.00000000000002132, 118.0000000000000142, -60.00000000000002132 ) ) ;
#3888 = AXIS2_PLACEMENT_3D ( 'NONE', #17191, #5509, #3757 ) ;
#3889 = LINE ( 'NONE', #18797, #9428 ) ;
#3890 = PLANE ( 'NONE',  #9263 ) ;
#3891 = ADVANCED_FACE ( 'NONE', ( #7656 ), #13622, .T. ) ;
#3892 = ORIENTED_EDGE ( 'NONE', *, *, #148, .T. ) ;
#3893 = ORIENTED_EDGE ( 'NONE', *, *, #3310, .F. ) ;
#3894 = EDGE_CURVE ( 'NONE', #15887, #1158, #16294, .T. ) ;
#3895 = CARTESIAN_POINT ( 'NONE',  ( -9.020235676060220698, -27.64274437364852588, 37.51367750791695244 ) ) ;
#3896 = SHAPE_REPRESENTATION_RELATIONSHIP ( 'NONE' , 'NONE' ,  #15908, #11089 ) ;
#3897 = ORIENTED_EDGE ( 'NONE', *, *, #15636, .F. ) ;
#3899 = VERTEX_POINT ( 'NONE', #208 ) ;
#3898 = ORIENTED_EDGE ( 'NONE', *, *, #2003, .F. ) ;
#3900 = CARTESIAN_POINT ( 'NONE',  ( -12.92450931948788906, -26.31681416490114245, 6.232427507916960430 ) ) ;
#3901 = CARTESIAN_POINT ( 'NONE',  ( -9.754982604823348780, -18.99630608921234654, 25.91992750791695599 ) ) ;
#3902 =( GEOMETRIC_REPRESENTATION_CONTEXT ( 3 ) GLOBAL_UNCERTAINTY_ASSIGNED_CONTEXT ( ( #241 ) ) GLOBAL_UNIT_ASSIGNED_CONTEXT ( ( #5755, #7124, #5955 ) ) REPRESENTATION_CONTEXT ( 'NONE', 'WORKASPACE' ) );
#3903 = VECTOR ( 'NONE', #3484, 1000.000000000000000 ) ;
#3904 = CARTESIAN_POINT ( 'NONE',  ( 2.500000000000000000, 1.178949249685212974, -2.042000000000001148 ) ) ;
#3905 = CARTESIAN_POINT ( 'NONE',  ( -1.767766952966370209, 65.76776695296638309, 49.20000000218494307 ) ) ;
#3906 = LINE ( 'NONE', #8325, #8745 ) ;
#3907 = ORIENTED_EDGE ( 'NONE', *, *, #258, .T. ) ;
#3908 = DIRECTION ( 'NONE',  ( 0.000000000000000000, 1.000000000000000000, 0.000000000000000000 ) ) ;
#3909 = VERTEX_POINT ( 'NONE', #7355 ) ;
#3910 = CARTESIAN_POINT ( 'NONE',  ( -25.00000000000000000, 53.00000000000000711, -25.49999999999999645 ) ) ;
#3911 = ORIENTED_EDGE ( 'NONE', *, *, #5520, .F. ) ;
#3912 = DIRECTION ( 'NONE',  ( -0.000000000000000000, 0.000000000000000000, 1.000000000000000000 ) ) ;
#3913 = CARTESIAN_POINT ( 'NONE',  ( 4.012830983233625304, 26.60336399182260791, 59.52836399182266547 ) ) ;
#3914 = DIRECTION ( 'NONE',  ( 0.5773502691896335026, 0.8164965809277204833, 0.000000000000000000 ) ) ;
#3915 = CARTESIAN_POINT ( 'NONE',  ( -0.8561741729129465073, 61.93301270000000613, 44.90000000109247225 ) ) ;
#3916 = CARTESIAN_POINT ( 'NONE',  ( -31.74999999999995737, 0.000000000000000000, 0.000000000000000000 ) ) ;
#3917 = AXIS2_PLACEMENT_3D ( 'NONE', #7492, #10521, #51 ) ;
#3918 = CARTESIAN_POINT ( 'NONE',  ( -41.00000000000000711, 110.0000000000000000, 8.000000000000000000 ) ) ;
#3919 = VECTOR ( 'NONE', #2853, 1000.000000000000000 ) ;
#3920 = CARTESIAN_POINT ( 'NONE',  ( 2.154726813346381942, 63.29944981661203229, 45.00000000000002842 ) ) ;
#3921 = EDGE_CURVE ( 'NONE', #9405, #11598, #10183, .T. ) ;
#3922 = ORIENTED_EDGE ( 'NONE', *, *, #19308, .F. ) ;
#3923 = ORIENTED_EDGE ( 'NONE', *, *, #9342, .T. ) ;
#3924 = CARTESIAN_POINT ( 'NONE',  ( -21.14459132904236327, -27.35725562635143149, 7.763677507916957765 ) ) ;
#3925 = LINE ( 'NONE', #11175, #1141 ) ;
#3926 = EDGE_LOOP ( 'NONE', ( #19216, #17342, #11741, #12693 ) ) ;
#3927 = CARTESIAN_POINT ( 'NONE',  ( -16.50457296725825174, -19.04416526290807354, 27.01757249208304046 ) ) ;
#3928 = CARTESIAN_POINT ( 'NONE',  ( -41.00000000000000711, 110.0000000000000000, -5.000000000000000888 ) ) ;
#3929 = EDGE_LOOP ( 'NONE', ( #12447, #17364, #11251, #16552 ) ) ;
#3930 = CARTESIAN_POINT ( 'NONE',  ( -12.92450931948790149, -21.68318583509881137, 38.39257249208304756 ) ) ;
#3931 = AXIS2_PLACEMENT_3D ( 'NONE', #5217, #1070, #13018 ) ;
#3932 = CARTESIAN_POINT ( 'NONE',  ( -41.00000000000000711, 110.0000000000000000, -44.00000000000000000 ) ) ;
#3933 = ORIENTED_EDGE ( 'NONE', *, *, #18463, .T. ) ;
#3934 = AXIS2_PLACEMENT_3D ( 'NONE', #16068, #17443, #1069 ) ;
#3935 = DIRECTION ( 'NONE',  ( 1.000000000000000000, 0.000000000000000000, -0.000000000000000000 ) ) ;
#3936 = PRODUCT_DEFINITION_SHAPE ( 'NONE', 'NONE',  #15783 ) ;
#3937 = ORIENTED_EDGE ( 'NONE', *, *, #4967, .F. ) ;
#3938 = FACE_OUTER_BOUND ( 'NONE', #1869, .T. ) ;
#3939 = CARTESIAN_POINT ( 'NONE',  ( -50.00000000000002132, 115.0000000000000000, 37.49999999999997868 ) ) ;
#3940 = DIRECTION ( 'NONE',  ( -2.602085213965211135E-16, 1.000000000000000000, -0.000000000000000000 ) ) ;
#3941 = EDGE_CURVE ( 'NONE', #3899, #13296, #2971, .T. ) ;
#3942 = CARTESIAN_POINT ( 'NONE',  ( -11.21908421996108629, -20.46040770435011069, 20.66992750791695244 ) ) ;
#3943 = PLANE ( 'NONE',  #2620 ) ;
#3944 = EDGE_CURVE ( 'NONE', #14005, #13130, #8720, .T. ) ;
#3945 = FACE_OUTER_BOUND ( 'NONE', #11031, .T. ) ;
#3946 = CARTESIAN_POINT ( 'NONE',  ( -25.00000000000000000, 53.00000000000000711, 30.00000000000000000 ) ) ;
#3947 = CIRCLE ( 'NONE', #19285, 0.2500000000000002220 ) ;
#3948 = DIRECTION ( 'NONE',  ( 0.000000000000000000, 0.000000000000000000, -1.000000000000000000 ) ) ;
#3949 = EDGE_LOOP ( 'NONE', ( #9113, #7233, #1762, #2647 ) ) ;
#3950 = VECTOR ( 'NONE', #12672, 1000.000000000000000 ) ;
#3951 = UNCERTAINTY_MEASURE_WITH_UNIT (LENGTH_MEASURE( 1.000000000000000082E-05 ), #4036, 'distance_accuracy_value', 'NONE');
#3952 = CARTESIAN_POINT ( 'NONE',  ( -19.24771351637089367, -21.35725562635142438, 34.88867750791696665 ) ) ;
#3953 = CARTESIAN_POINT ( 'NONE',  ( 0.8561741729129472844, 61.93301270000000613, 49.00000000109246656 ) ) ;
#3954 = CARTESIAN_POINT ( 'NONE',  ( -19.99999999999999645, -24.16482700510261949, 31.17382249208304046 ) ) ;
#3955 = DIRECTION ( 'NONE',  ( 0.000000000000000000, -1.000000000000000000, 0.000000000000000000 ) ) ;
#3956 = CARTESIAN_POINT ( 'NONE',  ( -2.499999999999992006, 62.96446609406726225, 46.15000000218496012 ) ) ;
#3957 = CARTESIAN_POINT ( 'NONE',  ( -17.35725562635144215, -19.58745947852648683, 24.82617750791695954 ) ) ;
#3958 = MANIFOLD_SOLID_BREP ( 'Cavity1', #7554 ) ;
#3959 = LINE ( 'NONE', #1316, #16106 ) ;
#3960 = AXIS2_PLACEMENT_3D ( 'NONE', #14333, #2468, #6799 ) ;
#3961 = CARTESIAN_POINT ( 'NONE',  ( -12.64274437364855252, -28.41254052147347053, 32.70117750791696665 ) ) ;
#3962 = LINE ( 'NONE', #7093, #18137 ) ;
#3963 = CARTESIAN_POINT ( 'NONE',  ( -20.04416526290809131, -22.82508104294700502, 36.64257249208304046 ) ) ;
#3964 = AXIS2_PLACEMENT_3D ( 'NONE', #15505, #6775, #2078 ) ;
#3965 = CARTESIAN_POINT ( 'NONE',  ( -1.035533905932738641, 66.50000000000000000, 49.85000000000000142 ) ) ;
#3966 = DIRECTION ( 'NONE',  ( 0.000000000000000000, 1.000000000000000000, 0.000000000000000000 ) ) ;
#3967 = EDGE_CURVE ( 'NONE', #16382, #13196, #18547, .T. ) ;
#3968 = CARTESIAN_POINT ( 'NONE',  ( -25.00000000000000711, 110.0000000000000000, 13.50000000000000000 ) ) ;
#3969 = CARTESIAN_POINT ( 'NONE',  ( 1.767766952966369987, 65.76776695296638309, 49.69999999999999574 ) ) ;
#3970 = CARTESIAN_POINT ( 'NONE',  ( 2.500000000000000000, 2.357898499370431722, -2.818925648462311528E-15 ) ) ;
#3971 = ORIENTED_EDGE ( 'NONE', *, *, #16201, .F. ) ;
#3972 = EDGE_CURVE ( 'NONE', #1793, #9810, #14912, .T. ) ;
#3973 = AXIS2_PLACEMENT_3D ( 'NONE', #99, #16171, #6081 ) ;
#3974 = PRESENTATION_STYLE_ASSIGNMENT (( #6726 ) ) ;
#3975 = CARTESIAN_POINT ( 'NONE',  ( 1.461580736456473684, 65.46158073645646880, 45.25000000109247367 ) ) ;
#3976 = CARTESIAN_POINT ( 'NONE',  ( -12.48433729119798130, -25.64274437364855075, 37.51367750791695954 ) ) ;
#3977 = CARTESIAN_POINT ( 'NONE',  ( -1.767766952966370209, 65.76776695296638309, 49.09999999999999432 ) ) ;
#3978 = CARTESIAN_POINT ( 'NONE',  ( -14.83517299489734853, -30.99999999999998224, 29.86132249208304046 ) ) ;
#3979 = CARTESIAN_POINT ( 'NONE',  ( -1.461580736456473906, 65.46158073645646880, 49.65000000109246514 ) ) ;
#3980 = ORIENTED_EDGE ( 'NONE', *, *, #11178, .T. ) ;
#3981 = CARTESIAN_POINT ( 'NONE',  ( -41.99999999999997868, 3.000000000000002665, -52.00000000000000000 ) ) ;
#3982 = CARTESIAN_POINT ( 'NONE',  ( 37.50000000000000711, -6.000000000000000000, -47.50000000000000000 ) ) ;
#3983 = CARTESIAN_POINT ( 'NONE',  ( 0.8561741729129460632, 66.06698730000000808, 46.10000000109246798 ) ) ;
#3984 = DIRECTION ( 'NONE',  ( 1.000000000000000000, -0.000000000000000000, -0.000000000000000000 ) ) ;
#3985 = DIRECTION ( 'NONE',  ( 0.000000000000000000, 0.000000000000000000, -1.000000000000000000 ) ) ;
#3986 = ADVANCED_FACE ( 'NONE', ( #1776 ), #3346, .F. ) ;
#3987 = CARTESIAN_POINT ( 'NONE',  ( 1.767766952966370653, 62.23223304703363112, 48.69999999999999574 ) ) ;
#3988 = EDGE_CURVE ( 'NONE', #10297, #18278, #9600, .T. ) ;
#3989 = FACE_OUTER_BOUND ( 'NONE', #15210, .T. ) ;
#3990 = VERTEX_POINT ( 'NONE', #9505 ) ;
#3991 = ORIENTED_EDGE ( 'NONE', *, *, #5773, .T. ) ;
#3992 = CARTESIAN_POINT ( 'NONE',  ( -14.83517299489734853, -30.99999999999998224, 3.611322492083039570 ) ) ;
#3993 =( NAMED_UNIT ( * ) SI_UNIT ( $, .STERADIAN. ) SOLID_ANGLE_UNIT ( ) );
#3994 = ORIENTED_EDGE ( 'NONE', *, *, #18190, .F. ) ;
#3996 = VERTEX_POINT ( 'NONE', #10683 ) ;
#3995 = ORIENTED_EDGE ( 'NONE', *, *, #2327, .T. ) ;
#3997 = CARTESIAN_POINT ( 'NONE',  ( -16.64274437364856496, -26.51566270880199738, 2.076177507916959986 ) ) ;
#3998 = CARTESIAN_POINT ( 'NONE',  ( -18.64274437364853654, -29.97976432393976509, 28.32617750791695954 ) ) ;
#3999 = DIRECTION ( 'NONE',  ( 0.000000000000000000, 0.000000000000000000, -1.000000000000000000 ) ) ;
#4000 = CARTESIAN_POINT ( 'NONE',  ( 2.500000000000002220, 62.96446609406726935, 47.25000000218494023 ) ) ;
#4001 = DIRECTION ( 'NONE',  ( -0.000000000000000000, 1.000000000000000000, -0.000000000000000000 ) ) ;
#4002 = EDGE_LOOP ( 'NONE', ( #10750, #10946, #7542, #17967 ) ) ;
#4003 = CARTESIAN_POINT ( 'NONE',  ( -41.00000000000000711, 110.0000000000000000, 21.00000000000000000 ) ) ;
#4004 = ORIENTED_EDGE ( 'NONE', *, *, #2274, .T. ) ;
#4005 = PLANE ( 'NONE',  #15346 ) ;
#4006 = ORIENTED_EDGE ( 'NONE', *, *, #6514, .T. ) ;
#4007 = CARTESIAN_POINT ( 'NONE',  ( 0.1249999999999895917, 32.14680374315353362, 54.33847763108504125 ) ) ;
#4008 = FACE_OUTER_BOUND ( 'NONE', #10455, .T. ) ;
#4009 = LINE ( 'NONE', #9882, #11875 ) ;
#4010 = CARTESIAN_POINT ( 'NONE',  ( -2.066987300000001415, 63.14382582708705627, 46.40000000109246514 ) ) ;
#4011 = EDGE_CURVE ( 'NONE', #14588, #16872, #3629, .T. ) ;
#4012 = CARTESIAN_POINT ( 'NONE',  ( -3.065533689247737392, -46.96461745799954457, 1.500000000000000000 ) ) ;
#4013 = CARTESIAN_POINT ( 'NONE',  ( -2.500000000000003553, 62.96446609406726225, 49.24999999999997868 ) ) ;
#4014 = DIRECTION ( 'NONE',  ( 0.000000000000000000, 0.000000000000000000, 1.000000000000000000 ) ) ;
#4015 = ORIENTED_EDGE ( 'NONE', *, *, #16920, .F. ) ;
#4016 = ORIENTED_EDGE ( 'NONE', *, *, #1632, .F. ) ;
#4017 = CARTESIAN_POINT ( 'NONE',  ( -18.53959229564986799, -20.21908421996107563, 40.35742750791696665 ) ) ;
#4018 = VECTOR ( 'NONE', #6437, 1000.000000000000000 ) ;
#4019 = DIRECTION ( 'NONE',  ( -0.000000000000000000, -0.000000000000000000, -1.000000000000000000 ) ) ;
#4020 = EDGE_LOOP ( 'NONE', ( #15496, #14883, #8830, #14322, #17070, #15793 ) ) ;
#4021 = CARTESIAN_POINT ( 'NONE',  ( -16.35725562635141372, -26.68048971390461332, 9.298822492083044011 ) ) ;
#4022 = CARTESIAN_POINT ( 'NONE',  ( 2.500000000000001776, 64.00000000000000000, 45.59999999999999432 ) ) ;
#4023 = ORIENTED_EDGE ( 'NONE', *, *, #8655, .T. ) ;
#4024 = CARTESIAN_POINT ( 'NONE',  ( -12.04416526290808420, -23.03132541760398766, 38.83007249208304756 ) ) ;
#4025 = DIRECTION ( 'NONE',  ( 1.000000000000000000, 0.000000000000000000, 0.000000000000000000 ) ) ;
#4026 = ORIENTED_EDGE ( 'NONE', *, *, #4115, .F. ) ;
#4027 = LINE ( 'NONE', #12754, #17835 ) ;
#4028 = EDGE_LOOP ( 'NONE', ( #18743, #6609, #16533, #16847 ) ) ;
#4029 = EDGE_CURVE ( 'NONE', #6116, #3066, #10772, .T. ) ;
#4030 = CARTESIAN_POINT ( 'NONE',  ( -24.00000000000000000, 53.00000000000000711, 1.500000000000001332 ) ) ;
#4031 = CARTESIAN_POINT ( 'NONE',  ( -37.50000000000002132, 0.000000000000000000, -25.00000000000002132 ) ) ;
#4032 = AXIS2_PLACEMENT_3D ( 'NONE', #13057, #15738, #11490 ) ;
#4033 = CARTESIAN_POINT ( 'NONE',  ( 1.035533905932739751, 61.50000000000000000, 47.95000000218494307 ) ) ;
#4034 = DIRECTION ( 'NONE',  ( 0.000000000000000000, 0.000000000000000000, 1.000000000000000000 ) ) ;
#4035 = CARTESIAN_POINT ( 'NONE',  ( -13.49542703274178379, -19.04416526290806289, 30.73242750791695599 ) ) ;
#4036 =( LENGTH_UNIT ( ) NAMED_UNIT ( * ) SI_UNIT ( .MILLI., .METRE. ) );
#4037 = EDGE_CURVE ( 'NONE', #12140, #7340, #13918, .T. ) ;
#4038 = CARTESIAN_POINT ( 'NONE',  ( -16.50457296725820555, -28.95583473709189448, 1.857427507916957765 ) ) ;
#4039 = AXIS2_PLACEMENT_3D ( 'NONE', #7139, #12823, #15691 ) ;
#4040 = CARTESIAN_POINT ( 'NONE',  ( -4.000000000000001776, 67.00000000000000000, 30.00000000000000000 ) ) ;
#4041 = VERTEX_POINT ( 'NONE', #3243 ) ;
#4042 = CARTESIAN_POINT ( 'NONE',  ( -12.35725562635140307, -28.24771351637085459, 8.423822492083042235 ) ) ;
#4043 = CARTESIAN_POINT ( 'NONE',  ( -21.95583473709191580, -21.95952864787954084, 8.419927507916955989 ) ) ;
#4044 = AXIS2_PLACEMENT_3D ( 'NONE', #3226, #16554, #3121 ) ;
#4045 = CARTESIAN_POINT ( 'NONE',  ( -0.8561741729129465073, 61.93301270000000613, 47.30000000109247082 ) ) ;
#4046 = CARTESIAN_POINT ( 'NONE',  ( -11.21908421996106320, -27.53959229564982181, 34.45507249208304046 ) ) ;
#4047 = CARTESIAN_POINT ( 'NONE',  ( -1.035533905932738863, 61.50000000000000000, 48.54999999999999716 ) ) ;
#4048 = VERTEX_POINT ( 'NONE', #15207 ) ;
#4049 = DIRECTION ( 'NONE',  ( 0.000000000000000000, -0.000000000000000000, -1.000000000000000000 ) ) ;
#4050 = CARTESIAN_POINT ( 'NONE',  ( -13.82508104294698192, -29.04416526290806644, 27.66992750791695244 ) ) ;
#4051 = MANIFOLD_SOLID_BREP ( 'Extrude-Thin1', #6669 ) ;
#4052 = LINE ( 'NONE', #8468, #9839 ) ;
#4054 = CARTESIAN_POINT ( 'NONE',  ( -32.50000000000001421, -6.000000000000000000, 24.99999999999998224 ) ) ;
#4053 = VECTOR ( 'NONE', #8211, 1000.000000000000000 ) ;
#4055 = LINE ( 'NONE', #5531, #7792 ) ;
#4056 = CARTESIAN_POINT ( 'NONE',  ( -14.83517299489735741, -28.99999999999998224, 35.11132249208304046 ) ) ;
#4057 = APPLICATION_CONTEXT ( 'automotive_design' ) ;
#4058 = CARTESIAN_POINT ( 'NONE',  ( -2.500000000000001776, 65.03553390593273775, 49.95000000000000284 ) ) ;
#4059 = CARTESIAN_POINT ( 'NONE',  ( 0.8561741729129471734, 61.93301270000000613, 49.20000000109247651 ) ) ;
#4060 = CIRCLE ( 'NONE', #19074, 2.041999999999999815 ) ;
#4061 = LINE ( 'NONE', #9751, #5852 ) ;
#4062 = CARTESIAN_POINT ( 'NONE',  ( -1.767766952966370209, 65.76776695296638309, 49.89999999999999147 ) ) ;
#4063 = DIRECTION ( 'NONE',  ( 0.000000000000000000, -0.4999999999999993894, 0.8660254037844389297 ) ) ;
#4064 = AXIS2_PLACEMENT_3D ( 'NONE', #3564, #2097, #7787 ) ;
#4065 = ORIENTED_EDGE ( 'NONE', *, *, #17882, .T. ) ;
#4066 = CARTESIAN_POINT ( 'NONE',  ( -0.8561741729129461742, 66.06698730000000808, 45.40000000109247225 ) ) ;
#4067 = CIRCLE ( 'NONE', #17529, 1.599999999999997202 ) ;
#4068 = CARTESIAN_POINT ( 'NONE',  ( -13.82508104294698192, -29.04416526290806644, 1.419927507916958209 ) ) ;
#4069 = CARTESIAN_POINT ( 'NONE',  ( 32.50000000000000000, 52.00000000000000711, -35.00000000000000000 ) ) ;
#4070 = CARTESIAN_POINT ( 'NONE',  ( -7.999999999999996447, -23.83517299489733432, 28.54882249208303691 ) ) ;
#4071 = AXIS2_PLACEMENT_3D ( 'NONE', #5795, #5997, #11854 ) ;
#4072 = ADVANCED_BREP_SHAPE_REPRESENTATION ( '', ( #10198, #1791 ), #3902 ) ;
#4073 = CARTESIAN_POINT ( 'NONE',  ( -2.066987300000001415, 63.14382582708705627, 47.40000000109247225 ) ) ;
#4074 = CARTESIAN_POINT ( 'NONE',  ( -16.64274437364856496, -26.51566270880199738, 33.57617750791696665 ) ) ;
#4075 = CARTESIAN_POINT ( 'NONE',  ( -19.99999999999999645, -23.83517299489738051, 8.201177507916957765 ) ) ;
#4076 = CARTESIAN_POINT ( 'NONE',  ( -40.00000000000000711, 113.0000000000000000, 30.00000000000000000 ) ) ;
#4077 = VECTOR ( 'NONE', #15130, 1000.000000000000000 ) ;
#4078 = CARTESIAN_POINT ( 'NONE',  ( 2.066987300000001859, 63.14382582708704916, 46.70000000109248361 ) ) ;
#4079 = DIRECTION ( 'NONE',  ( 1.000000000000000000, 0.000000000000000000, 0.000000000000000000 ) ) ;
#4080 = EDGE_CURVE ( 'NONE', #996, #12504, #7758, .T. ) ;
#4081 = ADVANCED_FACE ( 'NONE', ( #12914 ), #17339, .T. ) ;
#4082 = CARTESIAN_POINT ( 'NONE',  ( 1.767766952966370653, 62.23223304703363112, 47.89999999999999858 ) ) ;
#4083 = VECTOR ( 'NONE', #7387, 1000.000000000000000 ) ;
#4084 = CARTESIAN_POINT ( 'NONE',  ( -40.00000000000000711, 113.0000000000000000, 26.50000000000000000 ) ) ;
#4085 = EDGE_CURVE ( 'NONE', #5200, #8744, #13461, .T. ) ;
#4086 = AXIS2_PLACEMENT_3D ( 'NONE', #17442, #14400, #11644 ) ;
#4087 = LINE ( 'NONE', #16434, #4902 ) ;
#4088 = ORIENTED_EDGE ( 'NONE', *, *, #17527, .F. ) ;
#4089 = ORIENTED_EDGE ( 'NONE', *, *, #11323, .T. ) ;
#4090 = CARTESIAN_POINT ( 'NONE',  ( -20.00369391078757886, -29.24501739517668142, 9.517572492083038682 ) ) ;
#4091 = EDGE_CURVE ( 'NONE', #12028, #12628, #10065, .T. ) ;
#4092 = SURFACE_SIDE_STYLE ('',( #11337 ) ) ;
#4093 = ORIENTED_EDGE ( 'NONE', *, *, #18614, .T. ) ;
#4094 = VECTOR ( 'NONE', #1583, 1000.000000000000000 ) ;
#4096 = ORIENTED_EDGE ( 'NONE', *, *, #6380, .T. ) ;
#4095 = VERTEX_POINT ( 'NONE', #9693 ) ;
#4097 = CARTESIAN_POINT ( 'NONE',  ( -15.16482700510260706, -26.99999999999998579, 6.888677507916960430 ) ) ;
#4098 = CARTESIAN_POINT ( 'NONE',  ( -21.99999999999999289, -23.83517299489739116, 34.45117750791695954 ) ) ;
#4099 = CIRCLE ( 'NONE', #8479, 4.000000000000001776 ) ;
#4100 = DIRECTION ( 'NONE',  ( 1.000000000000000000, 0.000000000000000000, 0.000000000000000000 ) ) ;
#4101 = CARTESIAN_POINT ( 'NONE',  ( 2.066987300000002303, 63.14382582708705627, 48.30000000109247082 ) ) ;
#4102 = CARTESIAN_POINT ( 'NONE',  ( -41.00000000000000711, 53.00000000000000711, 13.50000000000000000 ) ) ;
#4103 = ORIENTED_EDGE ( 'NONE', *, *, #12131, .T. ) ;
#4104 = EDGE_CURVE ( 'NONE', #15084, #7321, #15686, .T. ) ;
#4105 = VECTOR ( 'NONE', #9537, 1000.000000000000000 ) ;
#4106 = CARTESIAN_POINT ( 'NONE',  ( -4.130991513055715103, 32.62172003681460808, 53.86292658466337713 ) ) ;
#4107 = VERTEX_POINT ( 'NONE', #19007 ) ;
#4108 = CARTESIAN_POINT ( 'NONE',  ( -25.00000000000000711, 53.00000000000000711, 20.00000000000000000 ) ) ;
#4109 = ORIENTED_EDGE ( 'NONE', *, *, #12877, .T. ) ;
#4110 = CARTESIAN_POINT ( 'NONE',  ( 1.844224359752661968, -41.39960408384398249, 3.000000000000000000 ) ) ;
#4111 = CARTESIAN_POINT ( 'NONE',  ( -31.74999999999995737, 1.836970198721030181E-16, -1.500000000000000222 ) ) ;
#4112 = DIRECTION ( 'NONE',  ( 0.000000000000000000, -1.000000000000000000, 0.000000000000000000 ) ) ;
#4113 = AXIS2_PLACEMENT_3D ( 'NONE', #13995, #3412, #18522 ) ;
#4114 = CARTESIAN_POINT ( 'NONE',  ( -0.8561741729129461742, 66.06698729999999387, 49.60000000109246798 ) ) ;
#4115 = EDGE_CURVE ( 'NONE', #4598, #2143, #2344, .T. ) ;
#4116 = DIRECTION ( 'NONE',  ( -0.000000000000000000, -0.000000000000000000, -1.000000000000000000 ) ) ;
#4117 = AXIS2_PLACEMENT_3D ( 'NONE', #5748, #16336, #16429 ) ;
#4118 = DIRECTION ( 'NONE',  ( 1.000000000000000000, -0.000000000000000000, -0.000000000000000000 ) ) ;
#4119 = CARTESIAN_POINT ( 'NONE',  ( 2.500000000000001776, 64.00000000000000000, 46.39999999999999858 ) ) ;
#4120 = ORIENTED_EDGE ( 'NONE', *, *, #17901, .F. ) ;
#4122 = VERTEX_POINT ( 'NONE', #11530 ) ;
#4121 = VERTEX_POINT ( 'NONE', #17251 ) ;
#4123 = CARTESIAN_POINT ( 'NONE',  ( -12.95952864787955150, -17.04416526290805933, -0.7675724920830436782 ) ) ;
#4124 =( BOUNDED_SURFACE ( )  B_SPLINE_SURFACE ( 1, 2, ( 
 ( #9701, #12358, #8063, #9418, #14125, #12266, #11167, #6490, #2263, #6589, #3355, #12454, #6682, #4928, #4831, #15412, #7867, #3637, #1980, #16783, #700, #9320, #7963, #14217, #5022, #5124, #10980, #410, #13928, #10885, #16880, #16985, #12556, #6395, #3544, #18356, #14023, #595, #11077, #17075, #9609, #15595, #12647, #18645, #5212, #17166, #3727, #15693, #6296, #10072, #875, #14309, #9884, #1164, #17440, #15974, #7141, #6854, #9973, #2440, #1067, #18733, #11256, #4010, #4209, #8334, #6952, #19014, #5484, #2537, #12827, #8520, #976, #11447, #13109, #5298, #9793, #8423, #15786, #11538, #17258, #18824, #5579, #12737, #14494, #17347, #16066, #2626, #5398, #784, #17536, #19109, #11354, #3915, #7044, #15878, #14595, #16162, #6771, #3826, #13014 ),
 ( #2732, #10161, #11642, #4114, #2351, #5682, #14399, #8611, #17633, #18917, #8703, #12923, #16458, #5873, #10661, #16556, #14688, #9103, #8904, #2926, #4706, #12036, #11835, #7243, #15092, #1266, #10369, #16662, #7435, #13512, #14891, #16255, #17832, #13305, #19305, #4408, #14986, #14796, #16363, #13214, #3025, #4308, #13403, #2828, #1367, #9002, #19205, #1466, #7336, #10265, #4609, #8809, #14522, #10564, #5975, #11944, #17936, #1665, #4507, #10463, #7638, #1561, #7537, #92, #6072, #5774, #11734, #18032, #18129, #3123, #13605, #188, #6174, #12136, #3227, #17731, #9386, #5182, #18233, #4808, #6462, #10757, #3520, #15383, #6655, #385, #16756, #16956, #11141, #10860, #1953, #16854, #7740, #3415, #17138, #9296, #6559, #8033, #2139, #7938, #13998 ) ),
 .UNSPECIFIED., .F., .F., .F. ) 
 B_SPLINE_SURFACE_WITH_KNOTS ( ( 2, 2 ),
 ( 3, 2, 2, 2, 2, 2, 2, 2, 2, 2, 2, 2, 2, 2, 2, 2, 2, 2, 2, 2, 2, 2, 2, 2, 2, 2, 2, 2, 2, 2, 2, 2, 2, 2, 2, 2, 2, 2, 2, 2, 2, 2, 2, 2, 2, 2, 2, 2, 2, 2, 3 ),
 ( 0.000000000000000000, 1.000000000000000000 ),
 ( 0.000000000000000000, 0.01785714285714285615, 0.03571428571428571230, 0.05357142857142856845, 0.07142857142857142461, 0.08928571428571428770, 0.1071428571428571369, 0.1250000000000000000, 0.1428571428571428492, 0.1607142857142857262, 0.1785714285714285754, 0.1964285714285714246, 0.2142857142857142738, 0.2321428571428571508, 0.2500000000000000000, 0.2678571428571428492, 0.2857142857142856984, 0.3035714285714285476, 0.3214285714285714524, 0.3392857142857143016, 0.3571428571428571508, 0.3750000000000000000, 0.3928571428571428492, 0.4107142857142856984, 0.4285714285714285476, 0.4464285714285714524, 0.4642857142857143016, 0.4821428571428571508, 0.5000000000000000000, 0.5178571428571429047, 0.5357142857142856984, 0.5535714285714286031, 0.5714285714285713969, 0.5892857142857143016, 0.6071428571428570953, 0.6250000000000000000, 0.6428571428571429047, 0.6607142857142856984, 0.6785714285714286031, 0.6964285714285713969, 0.7142857142857143016, 0.7321428571428570953, 0.7500000000000000000, 0.7678571428571429047, 0.7857142857142856984, 0.8035714285714286031, 0.8214285714285713969, 0.8392857142857143016, 0.8571428571428570953, 0.8750000000000000000, 0.8928571428571429047 ),
 .UNSPECIFIED. ) 
 GEOMETRIC_REPRESENTATION_ITEM ( )  RATIONAL_B_SPLINE_SURFACE ( (
 ( 1.000000000000000000, 0.9238795325112867385, 1.000000000000000000, 0.9238795325112867385, 1.000000000000000000, 0.9238795325112867385, 1.000000000000000000, 0.9238795325112867385, 1.000000000000000000, 0.9238795325112867385, 1.000000000000000000, 0.9238795325112867385, 1.000000000000000000, 0.9238795325112867385, 1.000000000000000000, 0.9238795325112867385, 1.000000000000000000, 0.9238795325112867385, 1.000000000000000000, 0.9238795325112867385, 1.000000000000000000, 0.9238795325112867385, 1.000000000000000000, 0.9238795325112867385, 1.000000000000000000, 0.9238795325112867385, 1.000000000000000000, 0.9238795325112867385, 1.000000000000000000, 0.9238795325112867385, 1.000000000000000000, 0.9238795325112867385, 1.000000000000000000, 0.9238795325112867385, 1.000000000000000000, 0.9238795325112867385, 1.000000000000000000, 0.9238795325112867385, 1.000000000000000000, 0.9238795325112867385, 1.000000000000000000, 0.9238795325112867385, 1.000000000000000000, 0.9238795325112867385, 1.000000000000000000, 0.9238795325112867385, 1.000000000000000000, 0.9238795325112867385, 1.000000000000000000, 0.9238795325112867385, 1.000000000000000000, 0.9238795325112867385, 1.000000000000000000, 0.9238795325112867385, 1.000000000000000000, 0.9238795325112867385, 1.000000000000000000, 0.9238795325112867385, 1.000000000000000000, 0.9238795325112867385, 1.000000000000000000, 0.9238795325112867385, 1.000000000000000000, 0.9238795325112867385, 1.000000000000000000, 0.9238795325112867385, 1.000000000000000000, 0.9238795325112867385, 1.000000000000000000, 0.9238795325112867385, 1.000000000000000000, 0.9238795325112867385, 1.000000000000000000, 0.9238795325112867385, 1.000000000000000000, 0.9238795325112867385, 1.000000000000000000, 0.9238795325112867385, 1.000000000000000000, 0.9238795325112867385, 1.000000000000000000, 0.9238795325112867385, 1.000000000000000000, 0.9238795325112867385, 1.000000000000000000, 0.9238795325112867385, 1.000000000000000000, 0.9238795325112867385, 1.000000000000000000, 0.9238795325112867385, 1.000000000000000000, 0.9238795325112867385, 1.000000000000000000, 0.9238795325112867385, 1.000000000000000000, 0.9238795325112867385, 1.000000000000000000, 0.9238795325112867385, 1.000000000000000000, 0.9238795325112867385, 1.000000000000000000),
 ( 1.000000000000000000, 0.9238795325112867385, 1.000000000000000000, 0.9238795325112867385, 1.000000000000000000, 0.9238795325112867385, 1.000000000000000000, 0.9238795325112867385, 1.000000000000000000, 0.9238795325112867385, 1.000000000000000000, 0.9238795325112867385, 1.000000000000000000, 0.9238795325112867385, 1.000000000000000000, 0.9238795325112867385, 1.000000000000000000, 0.9238795325112867385, 1.000000000000000000, 0.9238795325112867385, 1.000000000000000000, 0.9238795325112867385, 1.000000000000000000, 0.9238795325112867385, 1.000000000000000000, 0.9238795325112867385, 1.000000000000000000, 0.9238795325112867385, 1.000000000000000000, 0.9238795325112867385, 1.000000000000000000, 0.9238795325112867385, 1.000000000000000000, 0.9238795325112867385, 1.000000000000000000, 0.9238795325112867385, 1.000000000000000000, 0.9238795325112867385, 1.000000000000000000, 0.9238795325112867385, 1.000000000000000000, 0.9238795325112867385, 1.000000000000000000, 0.9238795325112867385, 1.000000000000000000, 0.9238795325112867385, 1.000000000000000000, 0.9238795325112867385, 1.000000000000000000, 0.9238795325112867385, 1.000000000000000000, 0.9238795325112867385, 1.000000000000000000, 0.9238795325112867385, 1.000000000000000000, 0.9238795325112867385, 1.000000000000000000, 0.9238795325112867385, 1.000000000000000000, 0.9238795325112867385, 1.000000000000000000, 0.9238795325112867385, 1.000000000000000000, 0.9238795325112867385, 1.000000000000000000, 0.9238795325112867385, 1.000000000000000000, 0.9238795325112867385, 1.000000000000000000, 0.9238795325112867385, 1.000000000000000000, 0.9238795325112867385, 1.000000000000000000, 0.9238795325112867385, 1.000000000000000000, 0.9238795325112867385, 1.000000000000000000, 0.9238795325112867385, 1.000000000000000000, 0.9238795325112867385, 1.000000000000000000, 0.9238795325112867385, 1.000000000000000000, 0.9238795325112867385, 1.000000000000000000, 0.9238795325112867385, 1.000000000000000000, 0.9238795325112867385, 1.000000000000000000, 0.9238795325112867385, 1.000000000000000000, 0.9238795325112867385, 1.000000000000000000, 0.9238795325112867385, 1.000000000000000000, 0.9238795325112867385, 1.000000000000000000, 0.9238795325112867385, 1.000000000000000000, 0.9238795325112867385, 1.000000000000000000) ) ) 
 REPRESENTATION_ITEM ( '' )  SURFACE ( )  );
#4125 = VECTOR ( 'NONE', #2259, 1000.000000000000000 ) ;
#4126 = FACE_OUTER_BOUND ( 'NONE', #4455, .T. ) ;
#4127 = ORIENTED_EDGE ( 'NONE', *, *, #15999, .F. ) ;
#4128 = CARTESIAN_POINT ( 'NONE',  ( -20.04416526290809131, -22.82508104294699791, 41.89257249208301914 ) ) ;
#4129 = EDGE_CURVE ( 'NONE', #3115, #7331, #5204, .T. ) ;
#4130 = EDGE_CURVE ( 'NONE', #2143, #7552, #14487, .T. ) ;
#4131 = LINE ( 'NONE', #14230, #5012 ) ;
#4132 = ORIENTED_EDGE ( 'NONE', *, *, #18875, .T. ) ;
#4133 = ADVANCED_FACE ( 'NONE', ( #968 ), #17524, .T. ) ;
#4134 = CARTESIAN_POINT ( 'NONE',  ( -17.99999999999999645, -24.16482700510260173, 41.67382249208304756 ) ) ;
#4135 = SURFACE_STYLE_FILL_AREA ( #3746 ) ;
#4136 = ORIENTED_EDGE ( 'NONE', *, *, #8424, .F. ) ;
#4137 = LINE ( 'NONE', #5231, #15040 ) ;
#4138 = ORIENTED_EDGE ( 'NONE', *, *, #18213, .F. ) ;
#4139 = PLANE ( 'NONE',  #5970 ) ;
#4140 = EDGE_CURVE ( 'NONE', #2146, #10091, #14210, .T. ) ;
#4141 = DIRECTION ( 'NONE',  ( -0.7071067811865562325, -0.4999999999999955036, 0.4999999999999924505 ) ) ;
#4142 = CIRCLE ( 'NONE', #16352, 1.500000000000001332 ) ;
#4143 = DIRECTION ( 'NONE',  ( -1.000000000000000000, -0.000000000000000000, -0.000000000000000000 ) ) ;
#4144 =( LENGTH_UNIT ( ) NAMED_UNIT ( * ) SI_UNIT ( .MILLI., .METRE. ) );
#4145 = DIRECTION ( 'NONE',  ( 0.000000000000000000, -0.000000000000000000, -1.000000000000000000 ) ) ;
#4146 = CARTESIAN_POINT ( 'NONE',  ( -11.46040770435012668, -27.78091578003887463, 21.98242750791695244 ) ) ;
#4147 = CARTESIAN_POINT ( 'NONE',  ( -24.00000000000000711, 110.0000000000000000, -18.00000000000000000 ) ) ;
#4148 = CARTESIAN_POINT ( 'NONE',  ( -9.999999999999994671, -24.16482700510257686, 5.576177507916958653 ) ) ;
#4149 = DIRECTION ( 'NONE',  ( 1.000000000000000000, 0.000000000000000000, 0.000000000000000000 ) ) ;
#4150 = ORIENTED_EDGE ( 'NONE', *, *, #7742, .F. ) ;
#4151 = ADVANCED_FACE ( 'NONE', ( #5289 ), #9785, .F. ) ;
#4152 = PRODUCT_DEFINITION_CONTEXT ( 'detailed design', #12696, 'design' ) ;
#4153 = CARTESIAN_POINT ( 'NONE',  ( -20.04416526290809131, -22.82508104294699791, 10.39257249208304223 ) ) ;
#4154 = CARTESIAN_POINT ( 'NONE',  ( -20.00369391078762860, -18.75498260482333279, 3.607427507916956433 ) ) ;
#4155 = CARTESIAN_POINT ( 'NONE',  ( 2.066987300000001415, 64.00000000000000000, 46.75000000109247367 ) ) ;
#4156 = CARTESIAN_POINT ( 'NONE',  ( -14.83517299489736985, -26.99999999999998579, 3.611322492083043123 ) ) ;
#4157 = CARTESIAN_POINT ( 'NONE',  ( -4.189607678530257395, 32.40336399182267257, 53.72836399182263278 ) ) ;
#4158 = ORIENTED_EDGE ( 'NONE', *, *, #3847, .F. ) ;
#4159 = CARTESIAN_POINT ( 'NONE',  ( -25.00000000000000000, 110.0000000000000000, 30.00000000000000000 ) ) ;
#4160 = CARTESIAN_POINT ( 'NONE',  ( -10.58745947852649927, -21.64274437364853654, 36.63867750791695954 ) ) ;
#4161 = FACE_OUTER_BOUND ( 'NONE', #14898, .T. ) ;
#4162 = CARTESIAN_POINT ( 'NONE',  ( -35.00000000000002132, -0.000000000000000000, -47.50000000000002132 ) ) ;
#4163 = CARTESIAN_POINT ( 'NONE',  ( -15.00000000000000000, 50.00000000000000711, 37.00000000000000000 ) ) ;
#4164 = CARTESIAN_POINT ( 'NONE',  ( -10.04416526290808598, -22.49542703274172695, 38.83007249208303335 ) ) ;
#4165 = PRODUCT_DEFINITION ( 'UNKNOWN', '', #15195, #4152 ) ;
#4166 = CARTESIAN_POINT ( 'NONE',  ( 1.035533905932739751, 61.50000000000000000, 47.85000000000000142 ) ) ;
#4167 = CARTESIAN_POINT ( 'NONE',  ( -40.00000000000000711, 53.00000000000000711, -37.50000000000000711 ) ) ;
#4168 = CARTESIAN_POINT ( 'NONE',  ( 44.99999999999997158, 6.000000000000000000, 55.00000000000000000 ) ) ;
#4169 = CARTESIAN_POINT ( 'NONE',  ( -1.461580736456473906, 65.46158073645646880, 45.65000000109247225 ) ) ;
#4170 = CARTESIAN_POINT ( 'NONE',  ( -43.50000000000000711, 118.0000000000000142, -52.50000000000000711 ) ) ;
#4171 = EDGE_CURVE ( 'NONE', #12791, #15600, #6945, .T. ) ;
#4172 = ORIENTED_EDGE ( 'NONE', *, *, #3494, .T. ) ;
#4173 = SHAPE_REPRESENTATION_RELATIONSHIP ( 'NONE' , 'NONE' ,  #8522, #6657 ) ;
#4174 = CARTESIAN_POINT ( 'NONE',  ( -14.83517299489739649, -18.99999999999997868, -0.9863224920830417908 ) ) ;
#4175 = CARTESIAN_POINT ( 'NONE',  ( -12.35725562635143682, -19.75228648362908501, -0.5488224920830419018 ) ) ;
#4176 = CARTESIAN_POINT ( 'NONE',  ( -2.499999999999999112, 65.03553390593273775, 49.15000000000000568 ) ) ;
#4177 = CARTESIAN_POINT ( 'NONE',  ( -17.35725562635140307, -28.41254052147349185, 9.298822492083040459 ) ) ;
#4178 = CARTESIAN_POINT ( 'NONE',  ( -0.8561741729129465073, 61.93301270000000613, 48.30000000109247082 ) ) ;
#4179 = CARTESIAN_POINT ( 'NONE',  ( -14.03132541760401786, -21.04416526290806289, 35.98242750791695954 ) ) ;
#4180 = CARTESIAN_POINT ( 'NONE',  ( -17.64274437364855430, -28.24771351637087236, 2.076177507916958209 ) ) ;
#4181 = CYLINDRICAL_SURFACE ( 'NONE', #5374, 2.750000000000000000 ) ;
#4182 = DIRECTION ( 'NONE',  ( -0.7071067811865335839, 0.000000000000000000, 0.7071067811865614505 ) ) ;
#4183 = DIRECTION ( 'NONE',  ( -1.000000000000000000, -0.000000000000000000, -2.081668171172167774E-16 ) ) ;
#4184 = DIRECTION ( 'NONE',  ( 0.000000000000000000, 0.000000000000000000, -1.000000000000000000 ) ) ;
#4185 = CARTESIAN_POINT ( 'NONE',  ( 1.461580736456473684, 65.46158073645646880, 49.45000000109246940 ) ) ;
#4186 = DIRECTION ( 'NONE',  ( 1.000000000000000000, 2.168404344971008868E-16, 0.000000000000000000 ) ) ;
#4187 = CARTESIAN_POINT ( 'NONE',  ( 2.500000000000001776, 64.00000000000000000, 44.90000000218493881 ) ) ;
#4188 = ORIENTED_EDGE ( 'NONE', *, *, #16499, .F. ) ;
#4189 = ORIENTED_EDGE ( 'NONE', *, *, #4915, .T. ) ;
#4190 = CARTESIAN_POINT ( 'NONE',  ( -9.754982604823302594, -29.00369391078756465, 2.955072492083039126 ) ) ;
#4191 = ORIENTED_EDGE ( 'NONE', *, *, #3664, .T. ) ;
#4192 = CARTESIAN_POINT ( 'NONE',  ( -2.500000000000003997, 65.03553390593273775, 47.55000000000000426 ) ) ;
#4194 = ORIENTED_EDGE ( 'NONE', *, *, #13010, .F. ) ;
#4193 = ORIENTED_EDGE ( 'NONE', *, *, #4980, .T. ) ;
#4195 = CARTESIAN_POINT ( 'NONE',  ( -12.31951028609537602, -22.64274437364854364, -0.1113224920830400977 ) ) ;
#4196 = CARTESIAN_POINT ( 'NONE',  ( -9.020235676060220698, -27.64274437364852588, 37.51367750791695244 ) ) ;
#4197 = PLANE ( 'NONE',  #12588 ) ;
#4198 = CARTESIAN_POINT ( 'NONE',  ( -2.066987300000001859, 64.85617417291294373, 48.70000000109247651 ) ) ;
#4199 = DIRECTION ( 'NONE',  ( 0.000000000000000000, 0.000000000000000000, -1.000000000000000000 ) ) ;
#4200 = EDGE_LOOP ( 'NONE', ( #10665, #7038 ) ) ;
#4201 = LINE ( 'NONE', #2726, #18205 ) ;
#4202 = ORIENTED_EDGE ( 'NONE', *, *, #21, .F. ) ;
#4203 = VECTOR ( 'NONE', #16316, 1000.000000000000000 ) ;
#4204 = ORIENTED_EDGE ( 'NONE', *, *, #3650, .F. ) ;
#4205 = CARTESIAN_POINT ( 'NONE',  ( 24.99999999999998579, 0.000000000000000000, 42.49999999999997868 ) ) ;
#4206 = DIRECTION ( 'NONE',  ( 0.000000000000000000, 0.000000000000000000, -1.000000000000000000 ) ) ;
#4207 = LINE ( 'NONE', #10160, #7489 ) ;
#4208 = EDGE_CURVE ( 'NONE', #513, #111, #15778, .T. ) ;
#4209 = CARTESIAN_POINT ( 'NONE',  ( -2.066987300000001415, 64.00000000000000000, 46.35000000109246798 ) ) ;
#4210 = CARTESIAN_POINT ( 'NONE',  ( -50.00000000000001421, 3.000000000000000000, 59.99999999999997868 ) ) ;
#4211 = CARTESIAN_POINT ( 'NONE',  ( -10.00000000000000000, 35.00000000000000000, 37.00000000000000000 ) ) ;
#4212 = DIRECTION ( 'NONE',  ( 0.000000000000000000, 0.5000000000000011102, 0.8660254037844380415 ) ) ;
#4213 = ORIENTED_EDGE ( 'NONE', *, *, #17059, .T. ) ;
#4215 = VERTEX_POINT ( 'NONE', #11347 ) ;
#4214 = EDGE_LOOP ( 'NONE', ( #9867, #9681 ) ) ;
#4216 = CARTESIAN_POINT ( 'NONE',  ( -8.044165262908075320, -26.04047135212042718, 5.794927507916956877 ) ) ;
#4217 = CARTESIAN_POINT ( 'NONE',  ( -25.00000000000000711, 53.00000000000000711, -12.50000000000000000 ) ) ;
#4218 = ORIENTED_EDGE ( 'NONE', *, *, #19229, .F. ) ;
#4219 = CIRCLE ( 'NONE', #12364, 1.599999999999997202 ) ;
#4220 = VERTEX_POINT ( 'NONE', #17433 ) ;
#4221 = CARTESIAN_POINT ( 'NONE',  ( -16.17491895705296656, -29.04416526290807710, 40.58007249208304046 ) ) ;
#4222 = EDGE_CURVE ( 'NONE', #14750, #12460, #9962, .T. ) ;
#4223 = FACE_OUTER_BOUND ( 'NONE', #6540, .T. ) ;
#4224 = VERTEX_POINT ( 'NONE', #14299 ) ;
#4225 = CARTESIAN_POINT ( 'NONE',  ( -17.51566270880199738, -25.64274437364856496, 41.23632249208304756 ) ) ;
#4226 = CARTESIAN_POINT ( 'NONE',  ( -7.999999999999986677, 60.00000000000000711, 45.00000000000000000 ) ) ;
#4227 = ORIENTED_EDGE ( 'NONE', *, *, #16848, .T. ) ;
#4228 = DIRECTION ( 'NONE',  ( 0.000000000000000000, 0.000000000000000000, -1.000000000000000000 ) ) ;
#4229 = VERTEX_POINT ( 'NONE', #11160 ) ;
#4230 = CARTESIAN_POINT ( 'NONE',  ( 32.50000000000000000, 52.00000000000000711, -37.50000000000000711 ) ) ;
#4231 = DIRECTION ( 'NONE',  ( 0.000000000000000000, -1.000000000000000000, 0.000000000000000000 ) ) ;
#4232 = DIRECTION ( 'NONE',  ( -0.000000000000000000, -1.000000000000000000, -0.000000000000000000 ) ) ;
#4233 = AXIS2_PLACEMENT_3D ( 'NONE', #13333, #6394, #9222 ) ;
#4234 = DIRECTION ( 'NONE',  ( 0.5773502691896311712, 0.8164965809277222597, 0.000000000000000000 ) ) ;
#4235 =( BOUNDED_CURVE ( )  B_SPLINE_CURVE ( 2, ( #2183, #12666, #6792, #5417, #3658, #15612, #8267 ),
 .UNSPECIFIED., .F., .F. ) 
 B_SPLINE_CURVE_WITH_KNOTS ( ( 3, 2, 2, 3 ),
 ( 0.7142857142857141906, 0.7321428571428569843, 0.7500000000000000000, 0.7678571432794591978 ),
 .UNSPECIFIED. ) 
 CURVE ( )  GEOMETRIC_REPRESENTATION_ITEM ( )  RATIONAL_B_SPLINE_CURVE ( ( 1.000000000000000444, 0.9238795325112862944, 1.000000000000000000, 0.9238795325112867385, 1.000000000000000000, 0.9238795325112867385, 1.000000000000000000 ) ) 
 REPRESENTATION_ITEM ( '' )  );
#4236 = ADVANCED_FACE ( 'NONE', ( #6760 ), #868, .T. ) ;
#4237 = CARTESIAN_POINT ( 'NONE',  ( -19.95583473709191580, -22.49542703274176603, 24.16992750791694888 ) ) ;
#4238 = EDGE_CURVE ( 'NONE', #16538, #10567, #18817, .T. ) ;
#4239 = CARTESIAN_POINT ( 'NONE',  ( 2.750000000000009770, 38.00000000000000000, 37.49999999999995737 ) ) ;
#4240 = EDGE_CURVE ( 'NONE', #6956, #2431, #7037, .T. ) ;
#4241 = CARTESIAN_POINT ( 'NONE',  ( -19.41254052147348830, -26.35725562635142083, 2.513677507916958209 ) ) ;
#4242 = DIRECTION ( 'NONE',  ( -1.000000000000000000, 0.000000000000000000, -9.251858538542970348E-17 ) ) ;
#4243 = ORIENTED_EDGE ( 'NONE', *, *, #9244, .F. ) ;
#4244 = CARTESIAN_POINT ( 'NONE',  ( -12.35725562635140307, -28.24771351637085459, 3.173822492083041347 ) ) ;
#4245 = VECTOR ( 'NONE', #7275, 1000.000000000000000 ) ;
#4246 = CARTESIAN_POINT ( 'NONE',  ( -13.28918265808472299, -31.04416526290805933, 1.419927507916956433 ) ) ;
#4247 = VECTOR ( 'NONE', #7524, 1000.000000000000000 ) ;
#4248 = CARTESIAN_POINT ( 'NONE',  ( -2.066987300000001859, 64.85617417291294373, 46.30000000109247082 ) ) ;
#4249 = CARTESIAN_POINT ( 'NONE',  ( -19.24771351637086880, -26.64274437364857206, 41.23632249208304046 ) ) ;
#4250 = FACE_OUTER_BOUND ( 'NONE', #11335, .T. ) ;
#4251 = ORIENTED_EDGE ( 'NONE', *, *, #2645, .F. ) ;
#4252 = CARTESIAN_POINT ( 'NONE',  ( -5.800000000000006928, 29.65425233947099315, 56.47747564417430510 ) ) ;
#4253 = CARTESIAN_POINT ( 'NONE',  ( -12.64274437364855252, -28.41254052147347053, 37.95117750791695954 ) ) ;
#4254 = CARTESIAN_POINT ( 'NONE',  ( -25.00000000000000000, 110.0000000000000000, 21.00000000000000355 ) ) ;
#4255 = CARTESIAN_POINT ( 'NONE',  ( -41.00000000000000711, 110.0000000000000000, -38.50000000000000711 ) ) ;
#4256 = FACE_OUTER_BOUND ( 'NONE', #14275, .T. ) ;
#4257 = CARTESIAN_POINT ( 'NONE',  ( -11.46040770435015332, -20.21908421996104011, 38.39257249208303335 ) ) ;
#4258 = EDGE_CURVE ( 'NONE', #4857, #9993, #4201, .T. ) ;
#4259 = CARTESIAN_POINT ( 'NONE',  ( 2.500000000000001776, 64.00000000000000000, 47.19999999999999574 ) ) ;
#4260 = CARTESIAN_POINT ( 'NONE',  ( 3.796994071234847710E-16, 61.93301269999999903, 45.95000000109246940 ) ) ;
#4261 = AXIS2_PLACEMENT_3D ( 'NONE', #2512, #18531, #5099 ) ;
#4262 = ADVANCED_FACE ( 'NONE', ( #5767 ), #8697, .F. ) ;
#4263 = VECTOR ( 'NONE', #3474, 1000.000000000000000 ) ;
#4264 =( NAMED_UNIT ( * ) PLANE_ANGLE_UNIT ( ) SI_UNIT ( $, .RADIAN. ) );
#4265 = CARTESIAN_POINT ( 'NONE',  ( -1.530808498934192803E-16, 66.50000000000000000, 45.79999999999999005 ) ) ;
#4266 = DIRECTION ( 'NONE',  ( -1.156482317317871725E-16, 0.000000000000000000, 1.000000000000000000 ) ) ;
#4267 = EDGE_LOOP ( 'NONE', ( #14611, #10667, #15284, #14682 ) ) ;
#4268 = CARTESIAN_POINT ( 'NONE',  ( 0.000000000000000000, 0.000000000000000000, 0.000000000000000000 ) ) ;
#4269 = CARTESIAN_POINT ( 'NONE',  ( -18.53959229564986799, -20.21908421996107563, 8.857427507916957765 ) ) ;
#4270 = CARTESIAN_POINT ( 'NONE',  ( -17.99999999999999645, -23.83517299489736985, 39.70117750791695954 ) ) ;
#4271 = CARTESIAN_POINT ( 'NONE',  ( -1.767766952966370209, 65.76776695296638309, 49.20000000218494307 ) ) ;
#4272 = CARTESIAN_POINT ( 'NONE',  ( -21.95583473709189803, -26.04047135212049469, 41.45507249208303335 ) ) ;
#4273 = CIRCLE ( 'NONE', #15542, 2.499999999999998668 ) ;
#4274 = VECTOR ( 'NONE', #13780, 1000.000000000000000 ) ;
#4275 = CARTESIAN_POINT ( 'NONE',  ( -0.8561741729129465073, 61.93301270000000613, 47.50000000109246656 ) ) ;
#4276 = CARTESIAN_POINT ( 'NONE',  ( -14.83517299489739649, -18.99999999999997868, 4.263677507916958653 ) ) ;
#4277 = CARTESIAN_POINT ( 'NONE',  ( -10.31147837279037738, -22.25502639194775512, -4.119453415160654225E-17 ) ) ;
#4278 = CARTESIAN_POINT ( 'NONE',  ( -41.00000000000000711, 110.0000000000000000, -11.50000000000000000 ) ) ;
#4279 = EDGE_CURVE ( 'NONE', #663, #7431, #14249, .T. ) ;
#4280 = LINE ( 'NONE', #16226, #9663 ) ;
#4281 = FACE_OUTER_BOUND ( 'NONE', #7993, .T. ) ;
#4282 = CYLINDRICAL_SURFACE ( 'NONE', #16332, 2.500000000000001776 ) ;
#4283 = CARTESIAN_POINT ( 'NONE',  ( 2.066987300000001415, 64.85617417291294373, 48.60000000109246798 ) ) ;
#4284 = CARTESIAN_POINT ( 'NONE',  ( -10.00000000000000000, 47.00000000000000711, 0.000000000000000000 ) ) ;
#4285 = AXIS2_PLACEMENT_3D ( 'NONE', #12655, #2448, #8259 ) ;
#4286 = VECTOR ( 'NONE', #14546, 1000.000000000000000 ) ;
#4287 = LINE ( 'NONE', #16045, #3004 ) ;
#4288 = ORIENTED_EDGE ( 'NONE', *, *, #17165, .T. ) ;
#4289 = EDGE_CURVE ( 'NONE', #12847, #17825, #1258, .T. ) ;
#4290 = ORIENTED_EDGE ( 'NONE', *, *, #10424, .F. ) ;
#4291 = CARTESIAN_POINT ( 'NONE',  ( -13.28918265808478694, -16.95583473709189093, 1.205072492083039126 ) ) ;
#4292 = CARTESIAN_POINT ( 'NONE',  ( -16.17491895705296656, -29.04416526290807354, 3.830072492083040903 ) ) ;
#4294 = ORIENTED_EDGE ( 'NONE', *, *, #15404, .F. ) ;
#4293 = ORIENTED_EDGE ( 'NONE', *, *, #4849, .F. ) ;
#4295 = CARTESIAN_POINT ( 'NONE',  ( -15.63902057219076269, -20.95583473709189448, 4.044927507916962206 ) ) ;
#4296 = CARTESIAN_POINT ( 'NONE',  ( -8.855408670957602979, -27.35725562635137820, 7.986322492083039570 ) ) ;
#4297 = DIRECTION ( 'NONE',  ( 0.000000000000000000, -0.000000000000000000, 1.000000000000000000 ) ) ;
#4298 = CARTESIAN_POINT ( 'NONE',  ( -1.530808498934192803E-16, 66.50000000000000000, 45.90000000218494591 ) ) ;
#4299 = ORIENTED_EDGE ( 'NONE', *, *, #2116, .T. ) ;
#4300 = ORIENTED_EDGE ( 'NONE', *, *, #1400, .T. ) ;
#4301 = CARTESIAN_POINT ( 'NONE',  ( -4.189131392896629613, 26.90500129688593134, 59.57932772728315030 ) ) ;
#4302 = ORIENTED_EDGE ( 'NONE', *, *, #8741, .T. ) ;
#4303 = ORIENTED_EDGE ( 'NONE', *, *, #10257, .T. ) ;
#4304 = DIRECTION ( 'NONE',  ( 0.000000000000000000, -1.000000000000000000, 0.000000000000000000 ) ) ;
#4305 = EDGE_CURVE ( 'NONE', #18807, #18025, #3117, .T. ) ;
#4306 = DIRECTION ( 'NONE',  ( 1.000000000000000000, -0.000000000000000000, -0.000000000000000000 ) ) ;
#4307 = LINE ( 'NONE', #7335, #7177 ) ;
#4308 = CARTESIAN_POINT ( 'NONE',  ( 2.066987300000002303, 63.14382582708705627, 47.70000000109247651 ) ) ;
#4309 = DIRECTION ( 'NONE',  ( 0.000000000000000000, 0.000000000000000000, -1.000000000000000000 ) ) ;
#4310 = DIRECTION ( 'NONE',  ( -1.000000000000000000, 0.000000000000000000, 0.000000000000000000 ) ) ;
#4311 = LINE ( 'NONE', #10467, #8937 ) ;
#4312 = ORIENTED_EDGE ( 'NONE', *, *, #5196, .F. ) ;
#4314 = ORIENTED_EDGE ( 'NONE', *, *, #13597, .T. ) ;
#4313 = ORIENTED_EDGE ( 'NONE', *, *, #2810, .T. ) ;
#4315 = CARTESIAN_POINT ( 'NONE',  ( -11.64274437364854187, -30.14459132904234195, 6.451177507916957765 ) ) ;
#4316 = CARTESIAN_POINT ( 'NONE',  ( 2.500000000000001776, 64.00000000000000000, 49.99999999999999289 ) ) ;
#4317 = ORIENTED_EDGE ( 'NONE', *, *, #18004, .T. ) ;
#4318 = ORIENTED_EDGE ( 'NONE', *, *, #18246, .T. ) ;
#4319 = CARTESIAN_POINT ( 'NONE',  ( -12.68318583509882380, -26.07549068051207541, 2.955072492083043123 ) ) ;
#4320 = CARTESIAN_POINT ( 'NONE',  ( -0.08838834764833139457, 29.68014068711926257, 56.80514068711929809 ) ) ;
#4321 = DIRECTION ( 'NONE',  ( 0.000000000000000000, -1.000000000000000000, 0.000000000000000000 ) ) ;
#4322 = VERTEX_POINT ( 'NONE', #7236 ) ;
#4323 = CARTESIAN_POINT ( 'NONE',  ( -18.04416526290808775, -23.36097942780924441, 41.89257249208304046 ) ) ;
#4324 = CARTESIAN_POINT ( 'NONE',  ( 2.500000000000001776, 65.03553390593273775, 47.35000000218494165 ) ) ;
#4325 = ORIENTED_EDGE ( 'NONE', *, *, #9152, .F. ) ;
#4326 = LINE ( 'NONE', #10284, #12826 ) ;
#4327 = VERTEX_POINT ( 'NONE', #8895 ) ;
#4328 = DIRECTION ( 'NONE',  ( 0.000000000000000000, 0.000000000000000000, -1.000000000000000000 ) ) ;
#4329 = LINE ( 'NONE', #1292, #2051 ) ;
#4330 = DIRECTION ( 'NONE',  ( 1.000000000000000000, 0.000000000000000000, 0.000000000000000000 ) ) ;
#4331 = APPLICATION_PROTOCOL_DEFINITION ( 'draft international standard', 'automotive_design', 1998, #9697 ) ;
#4332 = DIRECTION ( 'NONE',  ( 2.602085213965211135E-16, -1.000000000000000000, 0.000000000000000000 ) ) ;
#4333 = ADVANCED_FACE ( 'NONE', ( #10458 ), #2821, .F. ) ;
#4334 = EDGE_CURVE ( 'NONE', #16046, #5763, #1555, .T. ) ;
#4335 = VECTOR ( 'NONE', #5747, 1000.000000000000000 ) ;
#4336 = CARTESIAN_POINT ( 'NONE',  ( -13.49542703274178379, -19.04416526290806289, 20.23242750791696309 ) ) ;
#4338 = EDGE_CURVE ( 'NONE', #4981, #8044, #3018, .T. ) ;
#4337 = CARTESIAN_POINT ( 'NONE',  ( -21.50000000000000000, 115.0000000000000000, 32.50000000000000000 ) ) ;
#4339 = FACE_OUTER_BOUND ( 'NONE', #7454, .T. ) ;
#4340 = ORIENTED_EDGE ( 'NONE', *, *, #18991, .T. ) ;
#4341 = UNCERTAINTY_MEASURE_WITH_UNIT (LENGTH_MEASURE( 1.000000000000000082E-05 ), #4793, 'distance_accuracy_value', 'NONE');
#4342 = CARTESIAN_POINT ( 'NONE',  ( -17.35725562635140307, -28.41254052147349185, 4.048822492083041347 ) ) ;
#4343 = CARTESIAN_POINT ( 'NONE',  ( -7.955834737091916686, -22.28918265808470522, 0.1074275079169565300 ) ) ;
#4344 = CARTESIAN_POINT ( 'NONE',  ( -2.066987300000001415, 64.00000000000000000, 45.55000000109246372 ) ) ;
#4345 = CARTESIAN_POINT ( 'NONE',  ( -14.83517299489735741, -28.99999999999998224, 40.36132249208304046 ) ) ;
#4346 = VECTOR ( 'NONE', #1021, 1000.000000000000000 ) ;
#4347 = CARTESIAN_POINT ( 'NONE',  ( -7.499999999999994671, -38.00000000000000000, 4.500000000000000888 ) ) ;
#4348 = ORIENTED_EDGE ( 'NONE', *, *, #3519, .F. ) ;
#4349 = EDGE_CURVE ( 'NONE', #10567, #13006, #17626, .T. ) ;
#4350 = DIRECTION ( 'NONE',  ( -1.000000000000000000, 0.000000000000000000, 0.000000000000000000 ) ) ;
#4351 = ORIENTED_EDGE ( 'NONE', *, *, #9053, .F. ) ;
#4352 = CARTESIAN_POINT ( 'NONE',  ( 1.300000000000000044, -0.7390083445627225744, -1.279999999999999138 ) ) ;
#4353 = EDGE_CURVE ( 'NONE', #17254, #2217, #12488, .T. ) ;
#4354 = EDGE_CURVE ( 'NONE', #17877, #428, #6918, .T. ) ;
#4355 = CARTESIAN_POINT ( 'NONE',  ( 0.000000000000000000, -1.178949249685218970, -2.041999999999998039 ) ) ;
#4356 = LINE ( 'NONE', #8561, #15968 ) ;
#4357 = DIRECTION ( 'NONE',  ( 1.000000000000000000, 0.000000000000000000, -0.000000000000000000 ) ) ;
#4358 = CARTESIAN_POINT ( 'NONE',  ( -19.99999999999999645, -24.16482700510261949, 41.67382249208304046 ) ) ;
#4359 = CARTESIAN_POINT ( 'NONE',  ( 4.592425496802577917E-16, 61.50000000000000000, 47.79999999999999716 ) ) ;
#4360 = CARTESIAN_POINT ( 'NONE',  ( 1.461580736456473906, 62.53841926354353120, 46.05000000109246372 ) ) ;
#4361 = VECTOR ( 'NONE', #17532, 1000.000000000000000 ) ;
#4362 = CARTESIAN_POINT ( 'NONE',  ( 1.035533905932739751, 61.50000000000000000, 47.85000000000000142 ) ) ;
#4363 = CARTESIAN_POINT ( 'NONE',  ( 4.101219330881941794, 26.84264068711924267, 59.64264068711931088 ) ) ;
#4364 = AXIS2_PLACEMENT_3D ( 'NONE', #14840, #19352, #17886 ) ;
#4365 = ORIENTED_EDGE ( 'NONE', *, *, #2928, .T. ) ;
#4366 = CARTESIAN_POINT ( 'NONE',  ( -11.46040770435012668, -27.78091578003887463, 6.232427507916956877 ) ) ;
#4367 = CARTESIAN_POINT ( 'NONE',  ( -13.82508104294698192, -29.04416526290806644, 11.91992750791695421 ) ) ;
#4368 = CARTESIAN_POINT ( 'NONE',  ( -1.767766952966370209, 65.76776695296638309, 48.40000000218494591 ) ) ;
#4369 = CARTESIAN_POINT ( 'NONE',  ( -11.46040770435014977, -20.21908421996103655, 6.892572492083040459 ) ) ;
#4370 = AXIS2_PLACEMENT_3D ( 'NONE', #14648, #17691, #10124 ) ;
#4371 = EDGE_CURVE ( 'NONE', #17355, #8256, #8996, .T. ) ;
#4372 = EDGE_CURVE ( 'NONE', #11522, #6502, #86, .T. ) ;
#4373 = DIRECTION ( 'NONE',  ( -0.7071067811865486830, -0.5000000000000005551, 0.4999999999999978351 ) ) ;
#4374 = CARTESIAN_POINT ( 'NONE',  ( -15.16482700510259640, -28.99999999999998224, 6.888677507916957765 ) ) ;
#4375 = CARTESIAN_POINT ( 'NONE',  ( -9.955834737091912245, -22.82508104294696238, 10.60742750791695777 ) ) ;
#4376 = VECTOR ( 'NONE', #3843, 1000.000000000000000 ) ;
#4377 = DIRECTION ( 'NONE',  ( -0.000000000000000000, -1.000000000000000000, -0.000000000000000000 ) ) ;
#4378 = AXIS2_PLACEMENT_3D ( 'NONE', #7043, #18823, #13012 ) ;
#4379 = ADVANCED_FACE ( 'NONE', ( #4600 ), #10558, .F. ) ;
#4380 = DIRECTION ( 'NONE',  ( 0.000000000000000000, 0.000000000000000000, 1.000000000000000000 ) ) ;
#4381 = CARTESIAN_POINT ( 'NONE',  ( -10.00000000000000000, 35.00000000000000000, 33.99999999999999289 ) ) ;
#4382 = DIRECTION ( 'NONE',  ( 0.000000000000000000, 0.000000000000000000, -1.000000000000000000 ) ) ;
#4383 = AXIS2_PLACEMENT_3D ( 'NONE', #11244, #7035, #1155 ) ;
#4384 = CARTESIAN_POINT ( 'NONE',  ( 5.799326430397229615, 29.65377616443619857, 56.83055285973290438 ) ) ;
#4385 = DIRECTION ( 'NONE',  ( 0.000000000000000000, -1.000000000000000000, 0.000000000000000000 ) ) ;
#4386 = DIRECTION ( 'NONE',  ( 1.000000000000000000, -0.000000000000000000, -0.000000000000000000 ) ) ;
#4387 = EDGE_LOOP ( 'NONE', ( #16049, #4801, #18434, #10063 ) ) ;
#4388 = VERTEX_POINT ( 'NONE', #11045 ) ;
#4389 = CARTESIAN_POINT ( 'NONE',  ( -9.020235676060250896, -20.35725562635137820, 12.36132249208304046 ) ) ;
#4390 = CONICAL_SURFACE ( 'NONE', #16923, 5.800000000000005151, 0.7853981633974385090 ) ;
#4391 = CARTESIAN_POINT ( 'NONE',  ( 1.767766952966369987, 65.76776695296638309, 47.29999999999999716 ) ) ;
#4393 = VERTEX_POINT ( 'NONE', #4991 ) ;
#4392 = ORIENTED_EDGE ( 'NONE', *, *, #17824, .F. ) ;
#4394 = EDGE_CURVE ( 'NONE', #6468, #7257, #18324, .T. ) ;
#4395 = CARTESIAN_POINT ( 'NONE',  ( -16.35725562635142794, -21.31951028609535470, 14.32617750791695777 ) ) ;
#4396 = LINE ( 'NONE', #5960, #15216 ) ;
#4397 = CARTESIAN_POINT ( 'NONE',  ( -9.754982604823302594, -29.00369391078756465, 2.955072492083039126 ) ) ;
#4398 = CARTESIAN_POINT ( 'NONE',  ( 1.035533905932738197, 66.50000000000000000, 48.14999999999999858 ) ) ;
#4399 = CARTESIAN_POINT ( 'NONE',  ( 1.461580736456473906, 62.53841926354353120, 49.05000000109247082 ) ) ;
#4400 = EDGE_LOOP ( 'NONE', ( #18506, #15112, #16402, #3016, #13450 ) ) ;
#4401 = ORIENTED_EDGE ( 'NONE', *, *, #18393, .F. ) ;
#4402 = CARTESIAN_POINT ( 'NONE',  ( -4.130991513055792375, 26.86292658466339489, 59.62172003681457255 ) ) ;
#4403 = CARTESIAN_POINT ( 'NONE',  ( -12.50000000000000000, -35.50000000000000000, 5.500000000000000000 ) ) ;
#4404 = VERTEX_POINT ( 'NONE', #4803 ) ;
#4405 = CARTESIAN_POINT ( 'NONE',  ( -10.80184671977677091, -22.03375095468977207, 1.107186296610940968E-15 ) ) ;
#4406 = DIRECTION ( 'NONE',  ( 2.220446049250313081E-16, 0.7071067811865452413, 0.7071067811865497932 ) ) ;
#4407 = AXIS2_PLACEMENT_3D ( 'NONE', #10565, #4409, #17937 ) ;
#4408 = CARTESIAN_POINT ( 'NONE',  ( -0.8561741729129461742, 66.06698729999999387, 48.00000000109246656 ) ) ;
#4409 = DIRECTION ( 'NONE',  ( 0.000000000000000000, 0.000000000000000000, -1.000000000000000000 ) ) ;
#4410 = AXIS2_PLACEMENT_3D ( 'NONE', #11939, #14681, #17826 ) ;
#4411 = CARTESIAN_POINT ( 'NONE',  ( 1.844224359752661968, -41.39960408384398249, 1.500000000000000000 ) ) ;
#4412 = VERTEX_POINT ( 'NONE', #1949 ) ;
#4414 = EDGE_LOOP ( 'NONE', ( #10066, #12931, #8487, #6214 ) ) ;
#4413 = ORIENTED_EDGE ( 'NONE', *, *, #2516, .F. ) ;
#4415 = CARTESIAN_POINT ( 'NONE',  ( -7.955834737091916686, -22.28918265808470522, 15.85742750791695954 ) ) ;
#4416 = DIRECTION ( 'NONE',  ( -1.156482317317871725E-16, 0.000000000000000000, 1.000000000000000000 ) ) ;
#4417 = VECTOR ( 'NONE', #15037, 1000.000000000000000 ) ;
#4418 = EDGE_LOOP ( 'NONE', ( #8684, #4015, #16173, #12411 ) ) ;
#4419 = ORIENTED_EDGE ( 'NONE', *, *, #17019, .F. ) ;
#4420 = CARTESIAN_POINT ( 'NONE',  ( -11.99999999999999289, -23.83517299489735564, 7.548822492083043123 ) ) ;
#4421 = VECTOR ( 'NONE', #4186, 1000.000000000000000 ) ;
#4422 = DIRECTION ( 'NONE',  ( -0.000000000000000000, -1.000000000000000000, -0.000000000000000000 ) ) ;
#4423 = CARTESIAN_POINT ( 'NONE',  ( 44.99999999999997158, 0.000000000000000000, 53.40000000000000568 ) ) ;
#4424 = VERTEX_POINT ( 'NONE', #12327 ) ;
#4425 = CARTESIAN_POINT ( 'NONE',  ( -17.68048971390461688, -25.35725562635141372, 2.513677507916959986 ) ) ;
#4426 = DIRECTION ( 'NONE',  ( 1.000000000000000000, -0.000000000000000000, -0.000000000000000000 ) ) ;
#4427 = VERTEX_POINT ( 'NONE', #12426 ) ;
#4428 = AXIS2_PLACEMENT_3D ( 'NONE', #18521, #10948, #183 ) ;
#4429 = DIRECTION ( 'NONE',  ( 1.000000000000000000, -0.000000000000000000, -0.000000000000000000 ) ) ;
#4430 = PRODUCT_DEFINITION_SHAPE ( 'NONE', 'NONE',  #19398 ) ;
#4431 = ORIENTED_EDGE ( 'NONE', *, *, #15127, .F. ) ;
#4432 = CARTESIAN_POINT ( 'NONE',  ( -24.00000000000000000, 53.00000000000000711, -45.00000000000000000 ) ) ;
#4433 = DIRECTION ( 'NONE',  ( -1.000000000000000000, 0.000000000000000000, 0.000000000000000000 ) ) ;
#4434 = CARTESIAN_POINT ( 'NONE',  ( 37.49999999999999289, 0.000000000000000000, 47.49999999999997868 ) ) ;
#4435 = VECTOR ( 'NONE', #15280, 1000.000000000000000 ) ;
#4436 = APPLICATION_PROTOCOL_DEFINITION ( 'draft international standard', 'automotive_design', 1998, #3690 ) ;
#4437 = DIRECTION ( 'NONE',  ( 1.000000000000000000, -7.410738689372937262E-15, 7.410738689372897819E-15 ) ) ;
#4438 = AXIS2_PLACEMENT_3D ( 'NONE', #18478, #5046, #11008 ) ;
#4439 = LINE ( 'NONE', #1688, #10202 ) ;
#4440 = DIRECTION ( 'NONE',  ( -0.000000000000000000, 0.7071067811865456854, 0.7071067811865494601 ) ) ;
#4441 = CARTESIAN_POINT ( 'NONE',  ( -9.999999999999994671, -24.16482700510257686, 10.82617750791695777 ) ) ;
#4442 = FACE_OUTER_BOUND ( 'NONE', #10258, .T. ) ;
#4443 = ORIENTED_EDGE ( 'NONE', *, *, #3944, .T. ) ;
#4444 = CARTESIAN_POINT ( 'NONE',  ( -11.46040770435014977, -20.21908421996103655, 6.892572492083040459 ) ) ;
#4445 =( REPRESENTATION_RELATIONSHIP ('NONE','NONE', #7912, #7269 ) REPRESENTATION_RELATIONSHIP_WITH_TRANSFORMATION ( #7663 )SHAPE_REPRESENTATION_RELATIONSHIP( ) );
#4446 = AXIS2_PLACEMENT_3D ( 'NONE', #2564, #7273, #4145 ) ;
#4447 = CARTESIAN_POINT ( 'NONE',  ( 1.035533905932739751, 61.50000000000000000, 47.95000000218494307 ) ) ;
#4448 = ADVANCED_FACE ( 'NONE', ( #8029 ), #13797, .F. ) ;
#4449 = ADVANCED_FACE ( 'NONE', ( #6364 ), #15275, .T. ) ;
#4450 = CARTESIAN_POINT ( 'NONE',  ( -16.50457296725825174, -19.04416526290807354, 42.76757249208303335 ) ) ;
#4451 = AXIS2_PLACEMENT_3D ( 'NONE', #7178, #14630, #1194 ) ;
#4452 = CARTESIAN_POINT ( 'NONE',  ( -25.00000000000000000, 53.00000000000000711, 6.999999999999999112 ) ) ;
#4453 = EDGE_LOOP ( 'NONE', ( #7759, #12043, #971, #16465 ) ) ;
#4454 = CARTESIAN_POINT ( 'NONE',  ( -15.00000000000001954, -17.99999999999997868, -4.814824860968089633E-32 ) ) ;
#4455 = EDGE_LOOP ( 'NONE', ( #8696, #7850, #17555, #2737 ) ) ;
#4456 = DIRECTION ( 'NONE',  ( -1.000000000000000000, 0.000000000000000000, -0.000000000000000000 ) ) ;
#4457 = EDGE_CURVE ( 'NONE', #12613, #6640, #10854, .T. ) ;
#4458 = LINE ( 'NONE', #4759, #10788 ) ;
#4459 = CARTESIAN_POINT ( 'NONE',  ( -40.00000000000000711, 113.0000000000000000, 30.00000000000000000 ) ) ;
#4460 = DIRECTION ( 'NONE',  ( 0.000000000000000000, -0.7071067811865493491, 0.7071067811865457964 ) ) ;
#4461 = DIRECTION ( 'NONE',  ( 0.000000000000000000, 0.000000000000000000, -1.000000000000000000 ) ) ;
#4462 = CARTESIAN_POINT ( 'NONE',  ( -2.066987300000000971, 63.14382582708704916, 45.80000000109246372 ) ) ;
#4463 = ADVANCED_FACE ( 'NONE', ( #15469 ), #6261, .F. ) ;
#4464 = CARTESIAN_POINT ( 'NONE',  ( 0.000000000000000000, 1.478016689125442484, -1.626303258728256651E-15 ) ) ;
#4465 = CARTESIAN_POINT ( 'NONE',  ( 2.500000000000001776, 65.03553390593273775, 48.04999999999999716 ) ) ;
#4466 = DIRECTION ( 'NONE',  ( -0.000000000000000000, -0.000000000000000000, -1.000000000000000000 ) ) ;
#4467 = ORIENTED_EDGE ( 'NONE', *, *, #975, .F. ) ;
#4468 = DIRECTION ( 'NONE',  ( 0.000000000000000000, 0.000000000000000000, 1.000000000000000000 ) ) ;
#4469 = CARTESIAN_POINT ( 'NONE',  ( -13.49542703274178379, -19.04416526290806289, 4.482427507916957765 ) ) ;
#4470 = VECTOR ( 'NONE', #8030, 1000.000000000000000 ) ;
#4471 = CARTESIAN_POINT ( 'NONE',  ( -14.83517299489739649, -18.99999999999997868, 20.01367750791695954 ) ) ;
#4472 = CARTESIAN_POINT ( 'NONE',  ( -1.218482738863178705, 66.05435652614266928, 44.99999999999999289 ) ) ;
#4473 = EDGE_CURVE ( 'NONE', #6864, #201, #2494, .T. ) ;
#4474 = CARTESIAN_POINT ( 'NONE',  ( -16.17491895705296656, -29.04416526290807710, 3.830072492083041347 ) ) ;
#4475 = CARTESIAN_POINT ( 'NONE',  ( 1.461580736456473684, 65.46158073645646880, 45.45000000109246940 ) ) ;
#4476 = CARTESIAN_POINT ( 'NONE',  ( -19.41254052147348830, -26.35725562635142083, 7.763677507916958653 ) ) ;
#4477 = FACE_OUTER_BOUND ( 'NONE', #3320, .T. ) ;
#4478 = DIRECTION ( 'NONE',  ( 0.000000000000000000, -1.000000000000000000, 0.000000000000000000 ) ) ;
#4479 = DIRECTION ( 'NONE',  ( 1.156482317317871725E-16, -1.000000000000000000, 0.000000000000000000 ) ) ;
#4480 = DIRECTION ( 'NONE',  ( -1.000000000000000000, 0.000000000000000000, 0.000000000000000000 ) ) ;
#4481 = DIRECTION ( 'NONE',  ( -1.000000000000000000, -0.000000000000000000, -0.000000000000000000 ) ) ;
#4482 = FACE_OUTER_BOUND ( 'NONE', #7490, .T. ) ;
#4483 = CARTESIAN_POINT ( 'NONE',  ( -1.461580736456473462, 62.53841926354353120, 45.85000000109246798 ) ) ;
#4484 = LINE ( 'NONE', #1643, #5058 ) ;
#4485 = EDGE_CURVE ( 'NONE', #7631, #2980, #15375, .T. ) ;
#4486 = EDGE_CURVE ( 'NONE', #895, #11055, #10752, .T. ) ;
#4487 = DIRECTION ( 'NONE',  ( -0.000000000000000000, -0.000000000000000000, -1.000000000000000000 ) ) ;
#4488 = VERTEX_POINT ( 'NONE', #6168 ) ;
#4489 = EDGE_LOOP ( 'NONE', ( #469, #9331, #4934, #16736, #15181 ) ) ;
#4490 = EDGE_CURVE ( 'NONE', #14696, #10900, #13994, .T. ) ;
#4491 = CARTESIAN_POINT ( 'NONE',  ( -21.95583473709189803, -26.04047135212049469, 20.45507249208304046 ) ) ;
#4492 = CARTESIAN_POINT ( 'NONE',  ( -12.64274437364858628, -19.58745947852646552, 1.423822492083040903 ) ) ;
#4494 = EDGE_LOOP ( 'NONE', ( #16084, #8632, #3034 ) ) ;
#4493 = ORIENTED_EDGE ( 'NONE', *, *, #1811, .T. ) ;
#4495 = CARTESIAN_POINT ( 'NONE',  ( -14.36097942780923731, -27.04416526290806999, 22.41992750791696309 ) ) ;
#4496 = CARTESIAN_POINT ( 'NONE',  ( 4.592425496802577917E-16, 61.50000000000000000, 48.70000000218494307 ) ) ;
#4497 = CARTESIAN_POINT ( 'NONE',  ( -21.14459132904236327, -27.35725562635143149, 39.26367750791695244 ) ) ;
#4498 = DIRECTION ( 'NONE',  ( -0.000000000000000000, -0.7071067811865456854, -0.7071067811865494601 ) ) ;
#4499 = CARTESIAN_POINT ( 'NONE',  ( -1.530808498934192803E-16, 66.50000000000000000, 45.10000000218494165 ) ) ;
#4500 = ORIENTED_EDGE ( 'NONE', *, *, #9137, .F. ) ;
#4501 = ORIENTED_EDGE ( 'NONE', *, *, #16547, .T. ) ;
#4502 = CARTESIAN_POINT ( 'NONE',  ( 2.500000000000000000, 1.178949249685217193, 2.041999999999998483 ) ) ;
#4503 = DIRECTION ( 'NONE',  ( 0.000000000000000000, 0.000000000000000000, 1.000000000000000000 ) ) ;
#4504 = ORIENTED_EDGE ( 'NONE', *, *, #7119, .T. ) ;
#4505 = DIRECTION ( 'NONE',  ( 7.304098846218135653E-17, 0.000000000000000000, -1.000000000000000000 ) ) ;
#4506 = CARTESIAN_POINT ( 'NONE',  ( -41.00000000000000000, 47.00000000000000711, -50.00000000000000000 ) ) ;
#4507 = CARTESIAN_POINT ( 'NONE',  ( 1.461580736456473906, 62.53841926354353120, 46.85000000109246798 ) ) ;
#4508 = EDGE_CURVE ( 'NONE', #14672, #1673, #564, .T. ) ;
#4509 = EDGE_CURVE ( 'NONE', #14847, #14201, #6977, .T. ) ;
#4510 = CARTESIAN_POINT ( 'NONE',  ( 32.50000000000000000, 52.00000000000000711, 15.00000000000000000 ) ) ;
#4511 = LINE ( 'NONE', #3028, #6746 ) ;
#4512 = VERTEX_POINT ( 'NONE', #13599 ) ;
#4514 = ORIENTED_EDGE ( 'NONE', *, *, #12227, .F. ) ;
#4513 = ORIENTED_EDGE ( 'NONE', *, *, #10449, .F. ) ;
#4515 = CARTESIAN_POINT ( 'NONE',  ( -18.64274437364853654, -29.97976432393976509, 23.07617750791695954 ) ) ;
#4516 = DIRECTION ( 'NONE',  ( 1.000000000000000000, 0.000000000000000000, 0.000000000000000000 ) ) ;
#4517 = VERTEX_POINT ( 'NONE', #3222 ) ;
#4518 = ORIENTED_EDGE ( 'NONE', *, *, #11514, .F. ) ;
#4519 = CARTESIAN_POINT ( 'NONE',  ( -17.99999999999999645, -24.16482700510260173, 15.42382249208304223 ) ) ;
#4520 = STYLED_ITEM ( 'NONE', ( #8956 ), #16836 ) ;
#4521 = DIRECTION ( 'NONE',  ( 0.000000000000000000, 0.000000000000000000, -1.000000000000000000 ) ) ;
#4522 = CARTESIAN_POINT ( 'NONE',  ( 4.592425496802577917E-16, 61.50000000000000000, 47.10000000218494165 ) ) ;
#4523 = ORIENTED_EDGE ( 'NONE', *, *, #3273, .F. ) ;
#4524 = CARTESIAN_POINT ( 'NONE',  ( -12.31951028609537602, -22.64274437364854364, 10.38867750791695954 ) ) ;
#4525 = DIRECTION ( 'NONE',  ( -0.000000000000000000, -0.7071067811865456854, -0.7071067811865494601 ) ) ;
#4526 = ORIENTED_EDGE ( 'NONE', *, *, #16826, .F. ) ;
#4527 = FACE_OUTER_BOUND ( 'NONE', #15033, .T. ) ;
#4528 = ORIENTED_EDGE ( 'NONE', *, *, #132, .F. ) ;
#4529 = DIRECTION ( 'NONE',  ( -1.000000000000000000, 0.000000000000000000, -0.000000000000000000 ) ) ;
#4530 = DIRECTION ( 'NONE',  ( 1.047444401652940007E-14, 0.7071067811865495711, -0.7071067811865454633 ) ) ;
#4531 =( BOUNDED_CURVE ( )  B_SPLINE_CURVE ( 2, ( #3547, #7870, #505, #6492, #13837, #4930, #10887, #16881, #7664 ),
 .UNSPECIFIED., .F., .F. ) 
 B_SPLINE_CURVE_WITH_KNOTS ( ( 3, 2, 2, 2, 3 ),
 ( 0.000000000000000000, 0.01785714285714289085, 0.03571428571428578169, 0.05357142857142867254, 0.07142857142857156338 ),
 .UNSPECIFIED. ) 
 CURVE ( )  GEOMETRIC_REPRESENTATION_ITEM ( )  RATIONAL_B_SPLINE_CURVE ( ( 1.000000000000000000, 0.9238795325112867385, 1.000000000000000000, 0.9238795325112867385, 1.000000000000000000, 0.9238795325112867385, 1.000000000000000000, 0.9238795325112861834, 1.000000000000000666 ) ) 
 REPRESENTATION_ITEM ( '' )  );
#4532 = DIRECTION ( 'NONE',  ( 0.000000000000000000, -1.000000000000000000, 0.000000000000000000 ) ) ;
#4533 = EDGE_CURVE ( 'NONE', #11043, #6946, #3321, .T. ) ;
#4534 = SHAPE_DEFINITION_REPRESENTATION ( #2685, #15908 ) ;
#4535 = CARTESIAN_POINT ( 'NONE',  ( -9.183694056713489507E-15, 20.55025253169413091, 61.69238815542511389 ) ) ;
#4536 = CARTESIAN_POINT ( 'NONE',  ( -16.17491895705301275, -18.95583473709189803, 35.54492750791695954 ) ) ;
#4537 = VECTOR ( 'NONE', #6993, 1000.000000000000000 ) ;
#4538 = DIRECTION ( 'NONE',  ( -0.7071067811865463515, 0.5000000000000023315, -0.4999999999999994449 ) ) ;
#4539 = CARTESIAN_POINT ( 'NONE',  ( -12.64274437364855252, -28.41254052147347053, 22.20117750791695599 ) ) ;
#4540 = DIRECTION ( 'NONE',  ( 0.000000000000000000, -0.000000000000000000, -1.000000000000000000 ) ) ;
#4541 = EDGE_LOOP ( 'NONE', ( #6860, #3144, #17161, #6078, #1448 ) ) ;
#4542 = CARTESIAN_POINT ( 'NONE',  ( -11.46040770435014977, -20.21908421996103655, 22.64257249208303335 ) ) ;
#4543 = CARTESIAN_POINT ( 'NONE',  ( 1.461580736456473906, 62.53841926354353120, 45.85000000109246798 ) ) ;
#4544 = CARTESIAN_POINT ( 'NONE',  ( -18.04416526290808775, -23.36097942780924441, 10.39257249208304223 ) ) ;
#4545 = AXIS2_PLACEMENT_3D ( 'NONE', #7900, #143, #16516 ) ;
#4546 = DIRECTION ( 'NONE',  ( -0.000000000000000000, -1.000000000000000000, -0.000000000000000000 ) ) ;
#4547 = ORIENTED_EDGE ( 'NONE', *, *, #12722, .T. ) ;
#4548 = VECTOR ( 'NONE', #11488, 1000.000000000000000 ) ;
#4549 = LINE ( 'NONE', #10506, #15333 ) ;
#4550 = VERTEX_POINT ( 'NONE', #13696 ) ;
#4551 = PLANE ( 'NONE',  #8434 ) ;
#4552 = LINE ( 'NONE', #7684, #2039 ) ;
#4553 = PLANE ( 'NONE',  #11842 ) ;
#4554 = EDGE_CURVE ( 'NONE', #11338, #12423, #9290, .T. ) ;
#4555 = DIRECTION ( 'NONE',  ( 0.000000000000000000, 0.000000000000000000, -1.000000000000000000 ) ) ;
#4556 = ADVANCED_FACE ( 'NONE', ( #843 ), #12793, .F. ) ;
#4557 = CARTESIAN_POINT ( 'NONE',  ( -0.8561741729129461742, 66.06698730000000808, 47.20000000109246940 ) ) ;
#4558 = CARTESIAN_POINT ( 'NONE',  ( -12.70357423236093197, -43.78611686177728046, 1.500000000000000000 ) ) ;
#4559 = CARTESIAN_POINT ( 'NONE',  ( -1.767766952966370209, 65.76776695296638309, 45.89999999999999858 ) ) ;
#4560 = CARTESIAN_POINT ( 'NONE',  ( -1.265664690411616068E-16, 66.06698730000000808, 44.75000000109247367 ) ) ;
#4561 = CONICAL_SURFACE ( 'NONE', #11427, 0.7500000000000006661, 0.7853981633974511656 ) ;
#4562 = VECTOR ( 'NONE', #4633, 1000.000000000000114 ) ;
#4563 = ORIENTED_EDGE ( 'NONE', *, *, #15828, .T. ) ;
#4564 = CARTESIAN_POINT ( 'NONE',  ( -32.50000000000000000, 58.00000000000000000, -35.00000000000000000 ) ) ;
#4565 = CARTESIAN_POINT ( 'NONE',  ( -16.17491895705301275, -18.95583473709189803, 4.044927507916959541 ) ) ;
#4566 = CARTESIAN_POINT ( 'NONE',  ( -10.58745947852649927, -21.64274437364853654, 10.38867750791695777 ) ) ;
#4567 = CARTESIAN_POINT ( 'NONE',  ( 2.500000000000002220, 62.96446609406726935, 48.05000000218494449 ) ) ;
#4568 = CARTESIAN_POINT ( 'NONE',  ( -19.41254052147350961, -21.64274437364857562, 10.61132249208304046 ) ) ;
#4569 = CARTESIAN_POINT ( 'NONE',  ( -0.8561741729129465073, 61.93301270000000613, 45.90000000109247225 ) ) ;
#4570 = CARTESIAN_POINT ( 'NONE',  ( -17.64274437364855430, -28.24771351637087236, 7.326177507916957765 ) ) ;
#4571 = EDGE_CURVE ( 'NONE', #5689, #3132, #5949, .T. ) ;
#4572 = LINE ( 'NONE', #7906, #10476 ) ;
#4573 = VECTOR ( 'NONE', #17419, 1000.000000000000000 ) ;
#4574 = CARTESIAN_POINT ( 'NONE',  ( -19.95583473709191225, -22.49542703274176603, 18.91992750791695599 ) ) ;
#4575 = DIRECTION ( 'NONE',  ( -0.000000000000000000, -0.7071067811865456854, -0.7071067811865493491 ) ) ;
#4576 = VECTOR ( 'NONE', #14401, 1000.000000000000000 ) ;
#4577 = LINE ( 'NONE', #5746, #11537 ) ;
#4578 = DIRECTION ( 'NONE',  ( -1.000000000000000000, -0.000000000000000000, -0.000000000000000000 ) ) ;
#4579 = CARTESIAN_POINT ( 'NONE',  ( 47.00000000000000000, 6.000000000000000000, -56.99999999999999289 ) ) ;
#4580 = CARTESIAN_POINT ( 'NONE',  ( 1.461580736456473684, 65.46158073645646880, 45.45000000109246940 ) ) ;
#4581 = DIRECTION ( 'NONE',  ( 0.000000000000000000, 1.000000000000000000, 0.000000000000000000 ) ) ;
#4582 = ADVANCED_FACE ( 'NONE', ( #751 ), #6921, .T. ) ;
#4583 = CARTESIAN_POINT ( 'NONE',  ( -41.00000000000000711, 53.00000000000000711, -24.49999999999999645 ) ) ;
#4584 = ORIENTED_EDGE ( 'NONE', *, *, #10831, .F. ) ;
#4585 = ORIENTED_EDGE ( 'NONE', *, *, #4915, .F. ) ;
#4586 = CARTESIAN_POINT ( 'NONE',  ( -9.996306089212408708, -18.75498260482328661, 12.14257249208303691 ) ) ;
#4587 = VECTOR ( 'NONE', #6887, 1000.000000000000000 ) ;
#4588 = CONTEXT_DEPENDENT_SHAPE_REPRESENTATION ( #12072, #17558 ) ;
#4589 = VECTOR ( 'NONE', #16413, 1000.000000000000000 ) ;
#4590 = CARTESIAN_POINT ( 'NONE',  ( 0.000000000000000000, -32.00000000000000711, 1.500000000000000000 ) ) ;
#4592 = ORIENTED_EDGE ( 'NONE', *, *, #4508, .T. ) ;
#4591 = ORIENTED_EDGE ( 'NONE', *, *, #3546, .F. ) ;
#4593 = CARTESIAN_POINT ( 'NONE',  ( -11.95583473709191047, -23.36097942780921954, 10.60742750791695954 ) ) ;
#4594 = DIRECTION ( 'NONE',  ( 1.000000000000000000, -0.000000000000000000, 0.000000000000000000 ) ) ;
#4595 = CARTESIAN_POINT ( 'NONE',  ( -18.35725562635138886, -30.14459132904237393, 4.048822492083038682 ) ) ;
#4596 = CARTESIAN_POINT ( 'NONE',  ( 2.066987300000002303, 63.14382582708705627, 49.10000000109246088 ) ) ;
#4597 = CARTESIAN_POINT ( 'NONE',  ( 2.066987300000002303, 63.14382582708705627, 47.50000000109246656 ) ) ;
#4598 = VERTEX_POINT ( 'NONE', #3981 ) ;
#4599 = ORIENTED_EDGE ( 'NONE', *, *, #8394, .T. ) ;
#4600 = FACE_OUTER_BOUND ( 'NONE', #14380, .T. ) ;
#4601 = PLANE ( 'NONE',  #2890 ) ;
#4602 = ADVANCED_FACE ( 'NONE', ( #14466 ), #15757, .F. ) ;
#4603 = ORIENTED_EDGE ( 'NONE', *, *, #9391, .T. ) ;
#4604 = CARTESIAN_POINT ( 'NONE',  ( -14.55051906578255938, -19.99999999999997158, 5.135813185032623395E-31 ) ) ;
#4605 = FACE_OUTER_BOUND ( 'NONE', #8909, .T. ) ;
#4606 = EDGE_CURVE ( 'NONE', #4550, #3996, #12892, .T. ) ;
#4607 = ADVANCED_FACE ( 'NONE', ( #12615 ), #9764, .F. ) ;
#4608 = VECTOR ( 'NONE', #19314, 1000.000000000000000 ) ;
#4609 = CARTESIAN_POINT ( 'NONE',  ( -1.461580736456473906, 65.46158073645646880, 47.25000000109246656 ) ) ;
#4610 = VECTOR ( 'NONE', #3549, 1000.000000000000000 ) ;
#4611 = CARTESIAN_POINT ( 'NONE',  ( -15.00000000000000000, 47.00000000000000711, 33.99999999999999289 ) ) ;
#4612 = FACE_OUTER_BOUND ( 'NONE', #589, .T. ) ;
#4613 = ORIENTED_EDGE ( 'NONE', *, *, #616, .F. ) ;
#4615 = VERTEX_POINT ( 'NONE', #3696 ) ;
#4614 = VERTEX_POINT ( 'NONE', #5365 ) ;
#4616 = CARTESIAN_POINT ( 'NONE',  ( -12.95952864787955150, -17.04416526290805933, 20.23242750791695954 ) ) ;
#4617 = DIRECTION ( 'NONE',  ( 0.000000000000000000, 1.000000000000000000, 0.000000000000000000 ) ) ;
#4618 = B_SPLINE_CURVE_WITH_KNOTS ( 'NONE', 3,
 ( #11544, #11357, #6776, #15790 ),
 .UNSPECIFIED., .F., .F.,
 ( 4, 4 ),
 ( 0.000000000000000000, 1.000000000000000000 ),
 .UNSPECIFIED. ) ;
#4619 = ORIENTED_EDGE ( 'NONE', *, *, #13711, .T. ) ;
#4620 = ORIENTED_EDGE ( 'NONE', *, *, #7572, .T. ) ;
#4621 = CARTESIAN_POINT ( 'NONE',  ( -18.04416526290808775, -23.36097942780924441, 20.89257249208304046 ) ) ;
#4622 = VECTOR ( 'NONE', #4019, 1000.000000000000000 ) ;
#4623 = DIRECTION ( 'NONE',  ( 0.000000000000000000, 0.000000000000000000, -1.000000000000000000 ) ) ;
#4624 = LINE ( 'NONE', #4423, #2801 ) ;
#4625 = ORIENTED_EDGE ( 'NONE', *, *, #7838, .T. ) ;
#4626 = CARTESIAN_POINT ( 'NONE',  ( -13.35725562635142794, -21.48433729119796709, 20.45117750791696309 ) ) ;
#4627 = CARTESIAN_POINT ( 'NONE',  ( -40.00000000000000711, 110.0000000000000000, 30.00000000000000000 ) ) ;
#4628 = VERTEX_POINT ( 'NONE', #6734 ) ;
#4629 = EDGE_CURVE ( 'NONE', #11279, #6468, #11223, .T. ) ;
#4630 = CARTESIAN_POINT ( 'NONE',  ( 49.99999999999998579, 118.0000000000000142, 59.99999999999997868 ) ) ;
#4631 = VERTEX_POINT ( 'NONE', #5454 ) ;
#4632 = CARTESIAN_POINT ( 'NONE',  ( 44.99999999999998579, -1.285879139104706187E-16, -54.99999999999998579 ) ) ;
#4633 = DIRECTION ( 'NONE',  ( -2.775557561562890858E-16, 0.7071067811865456854, 0.7071067811865493491 ) ) ;
#4634 = CARTESIAN_POINT ( 'NONE',  ( -0.04166183285594760033, 33.84354264162095660, 52.64110397985704282 ) ) ;
#4635 = EDGE_CURVE ( 'NONE', #18570, #15994, #7013, .T. ) ;
#4636 = B_SPLINE_CURVE_WITH_KNOTS ( 'NONE', 3,
 ( #1526, #17900, #16217, #16418, #1330, #19268, #19363, #15051, #7400, #13471, #5931, #12094, #4472, #245, #7599, #13371, #2983, #8963 ),
 .UNSPECIFIED., .F., .F.,
 ( 4, 2, 2, 2, 2, 2, 2, 2, 4 ),
 ( 0.000000000000000000, 0.0005608035642034970908, 0.001121607128406994182, 0.001682410692610491381, 0.002243214256813988363, 0.002804017821017484695, 0.003364821385220981894, 0.003925624949424478226, 0.004486428513627974991 ),
 .UNSPECIFIED. ) ;
#4637 = DIRECTION ( 'NONE',  ( 1.000000000000000000, 0.000000000000000000, 0.000000000000000000 ) ) ;
#4638 = CARTESIAN_POINT ( 'NONE',  ( -1.767766952966369765, 62.23223304703363112, 46.20000000218494307 ) ) ;
#4639 = DIRECTION ( 'NONE',  ( -0.000000000000000000, 0.7071067811865497932, -0.7071067811865452413 ) ) ;
#4640 = DIRECTION ( 'NONE',  ( -1.000000000000000000, 0.000000000000000000, 0.000000000000000000 ) ) ;
#4641 = CARTESIAN_POINT ( 'NONE',  ( -20.04416526290808065, -25.17491895705300209, 13.23242750791695777 ) ) ;
#4642 = DIRECTION ( 'NONE',  ( 0.000000000000000000, 0.000000000000000000, 1.000000000000000000 ) ) ;
#4643 = VERTEX_POINT ( 'NONE', #12703 ) ;
#4644 = CARTESIAN_POINT ( 'NONE',  ( -17.64274437364858983, -19.75228648362910633, 16.29882249208304046 ) ) ;
#4645 = EDGE_CURVE ( 'NONE', #1661, #3528, #18790, .T. ) ;
#4646 = CARTESIAN_POINT ( 'NONE',  ( 0.8561741729129460632, 66.06698729999999387, 46.10000000109246798 ) ) ;
#4647 = CARTESIAN_POINT ( 'NONE',  ( -17.99999999999999645, -24.16482700510260173, 15.42382249208304223 ) ) ;
#4648 = LINE ( 'NONE', #4452, #3780 ) ;
#4649 = ORIENTED_EDGE ( 'NONE', *, *, #528, .F. ) ;
#4650 = CARTESIAN_POINT ( 'NONE',  ( -12.67132176431211832, -18.52296496192205311, 5.414424919715126740E-14 ) ) ;
#4651 = ORIENTED_EDGE ( 'NONE', *, *, #13942, .T. ) ;
#4652 = CARTESIAN_POINT ( 'NONE',  ( 2.500000000000000000, 2.357898499370431722, -2.818925648462311528E-15 ) ) ;
#4653 = DIRECTION ( 'NONE',  ( 0.000000000000000000, 0.000000000000000000, -1.000000000000000000 ) ) ;
#4654 = CARTESIAN_POINT ( 'NONE',  ( -47.00000000000001421, 6.000000000000000000, 56.99999999999997158 ) ) ;
#4655 = EDGE_CURVE ( 'NONE', #17673, #6113, #3883, .T. ) ;
#4656 = CARTESIAN_POINT ( 'NONE',  ( 0.8561741729129460632, 66.06698730000000808, 47.10000000109246798 ) ) ;
#4657 = CARTESIAN_POINT ( 'NONE',  ( 0.000000000000000000, 64.00000000000000000, 49.99999999999999289 ) ) ;
#4658 = CARTESIAN_POINT ( 'NONE',  ( 41.00000000000000000, 0.000000000000000000, -50.00000000000000000 ) ) ;
#4659 = VERTEX_POINT ( 'NONE', #14091 ) ;
#4660 = VECTOR ( 'NONE', #10338, 1000.000000000000000 ) ;
#4661 = CARTESIAN_POINT ( 'NONE',  ( 0.000000000000000000, 0.000000000000000000, 0.000000000000000000 ) ) ;
#4662 = CARTESIAN_POINT ( 'NONE',  ( -15.16482700510259640, -28.99999999999998224, 17.38867750791695599 ) ) ;
#4663 = CARTESIAN_POINT ( 'NONE',  ( -10.04416526290807710, -25.50457296725819489, 11.04492750791695421 ) ) ;
#4664 = PLANE ( 'NONE',  #16335 ) ;
#4665 = CARTESIAN_POINT ( 'NONE',  ( -16.17491895705296656, -29.04416526290807710, 24.83007249208304046 ) ) ;
#4666 = LINE ( 'NONE', #10623, #1325 ) ;
#4667 = CARTESIAN_POINT ( 'NONE',  ( -19.95583473709191580, -22.49542703274176603, 3.169927507916957321 ) ) ;
#4668 = DIRECTION ( 'NONE',  ( -1.000000000000000000, -0.000000000000000000, -0.000000000000000000 ) ) ;
#4670 = CARTESIAN_POINT ( 'NONE',  ( -14.83517299489739649, -18.99999999999997868, 25.26367750791695599 ) ) ;
#4669 = AXIS2_PLACEMENT_3D ( 'NONE', #17072, #7480, #498 ) ;
#4671 = CARTESIAN_POINT ( 'NONE',  ( -45.00000000000000000, -1.285879139104706187E-16, 54.99999999999998579 ) ) ;
#4672 = CARTESIAN_POINT ( 'NONE',  ( -25.00000000000000000, 53.00000000000000711, 30.00000000000000000 ) ) ;
#4673 = CARTESIAN_POINT ( 'NONE',  ( 0.8561741729129460632, 66.06698729999999387, 46.30000000109247082 ) ) ;
#4674 = FACE_OUTER_BOUND ( 'NONE', #1345, .T. ) ;
#4675 = CIRCLE ( 'NONE', #17487, 1.599999999999997202 ) ;
#4676 = DIRECTION ( 'NONE',  ( 0.000000000000000000, 1.000000000000000000, 0.000000000000000000 ) ) ;
#4677 = LINE ( 'NONE', #2903, #12097 ) ;
#4678 = FACE_OUTER_BOUND ( 'NONE', #16167, .T. ) ;
#4679 = CARTESIAN_POINT ( 'NONE',  ( 32.49999999999998579, -6.000000000000000000, -25.00000000000001421 ) ) ;
#4680 = CYLINDRICAL_SURFACE ( 'NONE', #16476, 2.500000000000001776 ) ;
#4681 = ORIENTED_EDGE ( 'NONE', *, *, #258, .F. ) ;
#4682 = ORIENTED_EDGE ( 'NONE', *, *, #16091, .F. ) ;
#4683 = CARTESIAN_POINT ( 'NONE',  ( -20.00369391078757886, -29.24501739517668142, 14.76757249208304046 ) ) ;
#4684 = AXIS2_PLACEMENT_3D ( 'NONE', #16526, #13273, #7506 ) ;
#4685 = CARTESIAN_POINT ( 'NONE',  ( -11.46040770435015332, -20.21908421996104011, 12.14257249208304046 ) ) ;
#4687 = VERTEX_POINT ( 'NONE', #11414 ) ;
#4686 = ORIENTED_EDGE ( 'NONE', *, *, #7810, .F. ) ;
#4688 = CARTESIAN_POINT ( 'NONE',  ( -13.64274437364856141, -26.68048971390460622, 16.95117750791696309 ) ) ;
#4689 = LINE ( 'NONE', #13591, #4247 ) ;
#4690 = CARTESIAN_POINT ( 'NONE',  ( -16.71081734191520596, -31.04416526290808065, 9.080072492083038682 ) ) ;
#4691 = AXIS2_PLACEMENT_3D ( 'NONE', #803, #9992, #9809 ) ;
#4692 = VECTOR ( 'NONE', #1848, 1000.000000000000000 ) ;
#4693 = CARTESIAN_POINT ( 'NONE',  ( -1.035533905932738641, 66.50000000000000000, 48.24999999999999289 ) ) ;
#4694 = CARTESIAN_POINT ( 'NONE',  ( 2.066987300000001859, 64.85617417291294373, 47.60000000109246798 ) ) ;
#4695 = ORIENTED_EDGE ( 'NONE', *, *, #11029, .T. ) ;
#4696 = VERTEX_POINT ( 'NONE', #15566 ) ;
#4697 = EDGE_CURVE ( 'NONE', #16767, #12626, #11519, .T. ) ;
#4698 = EDGE_CURVE ( 'NONE', #10838, #18337, #17227, .T. ) ;
#4699 = CARTESIAN_POINT ( 'NONE',  ( -41.00000000000000711, 110.0000000000000000, 0.5000000000000004441 ) ) ;
#4700 = CARTESIAN_POINT ( 'NONE',  ( 20.00000000000000355, -52.00000000000000711, 0.000000000000000000 ) ) ;
#4701 = ORIENTED_EDGE ( 'NONE', *, *, #15119, .F. ) ;
#4702 = CARTESIAN_POINT ( 'NONE',  ( 1.461580736456473684, 65.46158073645646880, 49.25000000109246656 ) ) ;
#4703 = CARTESIAN_POINT ( 'NONE',  ( -41.00000000000000711, 53.00000000000000711, -32.00000000000000000 ) ) ;
#4704 = EDGE_CURVE ( 'NONE', #12989, #7863, #2318, .T. ) ;
#4705 = CIRCLE ( 'NONE', #3434, 1.678500596222258556 ) ;
#4706 = CARTESIAN_POINT ( 'NONE',  ( -1.265664690411616068E-16, 66.06698730000000808, 48.75000000109246656 ) ) ;
#4707 = CARTESIAN_POINT ( 'NONE',  ( 2.500000000000000000, 0.000000000000000000, 0.000000000000000000 ) ) ;
#4708 = EDGE_CURVE ( 'NONE', #17355, #5403, #8390, .T. ) ;
#4709 = VECTOR ( 'NONE', #7557, 1000.000000000000000 ) ;
#4710 = CARTESIAN_POINT ( 'NONE',  ( 2.500000000000001776, 64.00000000000000000, 45.70000000218494307 ) ) ;
#4711 = ORIENTED_EDGE ( 'NONE', *, *, #14177, .F. ) ;
#4713 = EDGE_LOOP ( 'NONE', ( #9586, #4299, #5794, #4493 ) ) ;
#4712 = ORIENTED_EDGE ( 'NONE', *, *, #6424, .T. ) ;
#4714 = CARTESIAN_POINT ( 'NONE',  ( -7.999999999999996447, -24.16482700510256976, 16.07617750791695599 ) ) ;
#4715 = ORIENTED_EDGE ( 'NONE', *, *, #18463, .F. ) ;
#4716 = VECTOR ( 'NONE', #13153, 1000.000000000000000 ) ;
#4717 = ORIENTED_EDGE ( 'NONE', *, *, #1092, .T. ) ;
#4718 = CARTESIAN_POINT ( 'NONE',  ( -17.31681416490117087, -21.92450931948788551, 16.08007249208304401 ) ) ;
#4719 = EDGE_CURVE ( 'NONE', #10078, #5590, #9712, .T. ) ;
#4720 = CARTESIAN_POINT ( 'NONE',  ( -18.78091578003889950, -27.53959229564985378, 39.04492750791695954 ) ) ;
#4721 = VECTOR ( 'NONE', #13894, 1000.000000000000000 ) ;
#4722 = DIRECTION ( 'NONE',  ( 1.000000000000000000, -0.000000000000000000, -0.000000000000000000 ) ) ;
#4723 = ORIENTED_EDGE ( 'NONE', *, *, #19188, .T. ) ;
#4724 = CARTESIAN_POINT ( 'NONE',  ( -17.99999999999999645, -23.83517299489736985, 13.45117750791696309 ) ) ;
#4725 = VECTOR ( 'NONE', #6268, 1000.000000000000000 ) ;
#4726 = DIRECTION ( 'NONE',  ( 0.000000000000000000, 0.000000000000000000, 1.000000000000000000 ) ) ;
#4727 = VERTEX_POINT ( 'NONE', #2408 ) ;
#4728 = CARTESIAN_POINT ( 'NONE',  ( 4.592425496802577917E-16, 61.50000000000000000, 45.39999999999999858 ) ) ;
#4729 = ORIENTED_EDGE ( 'NONE', *, *, #2528, .F. ) ;
#4730 = EDGE_CURVE ( 'NONE', #375, #3539, #19058, .T. ) ;
#4731 = CARTESIAN_POINT ( 'NONE',  ( -21.50000000000000000, 118.0000000000000142, -52.50000000000000711 ) ) ;
#4732 = DIRECTION ( 'NONE',  ( -2.775557561562883462E-16, 0.7071067811865454633, 0.7071067811865495711 ) ) ;
#4733 = CARTESIAN_POINT ( 'NONE',  ( -0.08332366571188480620, 33.84322526524066177, 52.64078660347674798 ) ) ;
#4734 = STYLED_ITEM ( 'NONE', ( #6506 ), #3611 ) ;
#4735 = LINE ( 'NONE', #16689, #14597 ) ;
#4736 = CARTESIAN_POINT ( 'NONE',  ( -0.9999999999999945599, -28.00000000000000000, 4.500000000000000888 ) ) ;
#4737 = VECTOR ( 'NONE', #17814, 1000.000000000000000 ) ;
#4738 = CARTESIAN_POINT ( 'NONE',  ( -4.042620306204127267, 26.80012125920696064, 59.68389060951041358 ) ) ;
#4739 = DIRECTION ( 'NONE',  ( 0.000000000000000000, 0.000000000000000000, -1.000000000000000000 ) ) ;
#4740 = EDGE_LOOP ( 'NONE', ( #18121, #19348, #12434, #16593 ) ) ;
#4741 = CARTESIAN_POINT ( 'NONE',  ( -18.78091578003889950, -27.53959229564985378, 12.79492750791695421 ) ) ;
#4742 = VECTOR ( 'NONE', #16338, 1000.000000000000000 ) ;
#4743 = DIRECTION ( 'NONE',  ( 0.000000000000000000, -1.000000000000000000, 0.000000000000000000 ) ) ;
#4744 = EDGE_CURVE ( 'NONE', #17457, #8804, #13376, .T. ) ;
#4745 = ORIENTED_EDGE ( 'NONE', *, *, #14636, .F. ) ;
#4746 = EDGE_CURVE ( 'NONE', #17457, #12847, #2700, .T. ) ;
#4747 = CARTESIAN_POINT ( 'NONE',  ( -13.82508104294702100, -18.95583473709188382, 11.70507249208303868 ) ) ;
#4748 = EDGE_CURVE ( 'NONE', #14224, #13312, #235, .T. ) ;
#4749 = VECTOR ( 'NONE', #776, 1000.000000000000000 ) ;
#4750 = CARTESIAN_POINT ( 'NONE',  ( -1.040834085586084257E-14, 34.69238815542512100, 47.55025253169419841 ) ) ;
#4751 = EDGE_CURVE ( 'NONE', #14672, #19394, #2876, .T. ) ;
#4752 = CARTESIAN_POINT ( 'NONE',  ( -12.04416526290808420, -23.03132541760398766, 17.83007249208304046 ) ) ;
#4753 = CARTESIAN_POINT ( 'NONE',  ( 2.500000000000000000, 2.500728763858895382E-16, -2.041999999999999815 ) ) ;
#4754 = ORIENTED_EDGE ( 'NONE', *, *, #15964, .F. ) ;
#4755 = AXIS2_PLACEMENT_3D ( 'NONE', #13630, #2951, #10491 ) ;
#4756 = LINE ( 'NONE', #10901, #18774 ) ;
#4757 = ORIENTED_EDGE ( 'NONE', *, *, #805, .T. ) ;
#4758 = CARTESIAN_POINT ( 'NONE',  ( -41.99999999999997868, 139.6861997365471950, 51.99999999999997868 ) ) ;
#4759 = CARTESIAN_POINT ( 'NONE',  ( 37.50000000000000711, -6.000000000000000000, -45.00000000000000000 ) ) ;
#4760 = VECTOR ( 'NONE', #14395, 1000.000000000000000 ) ;
#4761 = DIRECTION ( 'NONE',  ( 0.000000000000000000, -0.000000000000000000, -1.000000000000000000 ) ) ;
#4762 = FACE_OUTER_BOUND ( 'NONE', #4713, .T. ) ;
#4763 = AXIS2_PLACEMENT_3D ( 'NONE', #7503, #1432, #7407 ) ;
#4764 = EDGE_CURVE ( 'NONE', #4322, #12056, #7186, .T. ) ;
#4765 = PRESENTATION_STYLE_ASSIGNMENT (( #6222 ) ) ;
#4766 = CARTESIAN_POINT ( 'NONE',  ( 21.50000000000001421, 2.999000000000001442, 32.49999999999998579 ) ) ;
#4767 = CARTESIAN_POINT ( 'NONE',  ( -12.50000000000000000, -35.50000000000000000, 5.500000000000000000 ) ) ;
#4768 = AXIS2_PLACEMENT_3D ( 'NONE', #10193, #1186, #19233 ) ;
#4769 = ORIENTED_EDGE ( 'NONE', *, *, #10982, .T. ) ;
#4770 =( BOUNDED_SURFACE ( )  B_SPLINE_SURFACE ( 1, 2, ( 
 ( #10453, #3014, #6164, #8990, #18223, #6360, #17821, #14977, #8891, #4596, #18119, #10554, #10650, #4799, #3218, #14881, #9190, #7426, #15178, #16745, #9285, #1655, #13393, #1453, #7730, #1746, #19389, #1840, #3113, #9093, #7629, #15754, #7927, #2226, #5264, #6454, #8115, #1945, #2130, #12612, #8217, #560, #8025, #6550, #14088, #12516, #16844, #11041, #6647, #17039, #841, #3406, #13990, #662, #18517, #12701, #5085, #12323, #14184, #2032, #3596, #9569, #9377, #3693, #15562, #15655, #18319, #18607, #2316, #13890, #5171, #11134, #15371, #749, #3794, #12421, #10944, #18419, #17130, #9664, #6732, #18702, #11220, #17225, #9761, #8299, #466, #14274, #4889, #4985, #10850, #16946, #3510, #9478, #15464, #2792, #15934, #12980, #16221, #8388, #11411 ),
 ( #18788, #16037, #3979, #2697, #2500, #8672, #11702, #8486, #19171, #14362, #937, #8578, #6919, #1224, #8769, #6822, #12890, #5363, #18889, #14654, #14760, #10040, #11605, #2597, #15844, #1036, #7011, #17601, #14557, #4178, #9937, #12790, #11322, #5548, #17317, #3880, #11504, #2406, #17695, #5452, #5645, #17496, #1131, #17407, #13072, #4275, #14464, #4073, #10235, #9846, #18981, #7110, #10130, #19071, #16126, #7206, #13179, #5742, #17903, #16625, #16420, #3191, #6231, #2985, #13667, #8869, #14854, #3084, #1427, #15150, #16720, #1332, #7404, #19270, #13373, #9165, #3290, #4569, #6135, #16521, #10332, #14954, #1528, #12098, #10528, #18094, #4475, #7302, #9260, #58, #10427, #7603, #17996, #13269, #7498, #8967, #1720, #7700, #13474, #6041, #5841 ) ),
 .UNSPECIFIED., .F., .F., .F. ) 
 B_SPLINE_SURFACE_WITH_KNOTS ( ( 2, 2 ),
 ( 3, 2, 2, 2, 2, 2, 2, 2, 2, 2, 2, 2, 2, 2, 2, 2, 2, 2, 2, 2, 2, 2, 2, 2, 2, 2, 2, 2, 2, 2, 2, 2, 2, 2, 2, 2, 2, 2, 2, 2, 2, 2, 2, 2, 2, 2, 2, 2, 2, 2, 3 ),
 ( 0.000000000000000000, 1.000000000000000000 ),
 ( 0.000000000000000000, 0.01785714285714285615, 0.03571428571428571230, 0.05357142857142856845, 0.07142857142857142461, 0.08928571428571428770, 0.1071428571428571369, 0.1250000000000000000, 0.1428571428571428492, 0.1607142857142857262, 0.1785714285714285754, 0.1964285714285714246, 0.2142857142857142738, 0.2321428571428571508, 0.2500000000000000000, 0.2678571428571428492, 0.2857142857142856984, 0.3035714285714285476, 0.3214285714285714524, 0.3392857142857143016, 0.3571428571428571508, 0.3750000000000000000, 0.3928571428571428492, 0.4107142857142856984, 0.4285714285714285476, 0.4464285714285714524, 0.4642857142857143016, 0.4821428571428571508, 0.5000000000000000000, 0.5178571428571429047, 0.5357142857142856984, 0.5535714285714286031, 0.5714285714285713969, 0.5892857142857143016, 0.6071428571428570953, 0.6250000000000000000, 0.6428571428571429047, 0.6607142857142856984, 0.6785714285714286031, 0.6964285714285713969, 0.7142857142857143016, 0.7321428571428570953, 0.7500000000000000000, 0.7678571428571429047, 0.7857142857142856984, 0.8035714285714286031, 0.8214285714285713969, 0.8392857142857143016, 0.8571428571428570953, 0.8750000000000000000, 0.8928571428571429047 ),
 .UNSPECIFIED. ) 
 GEOMETRIC_REPRESENTATION_ITEM ( )  RATIONAL_B_SPLINE_SURFACE ( (
 ( 1.000000000000000000, 0.9238795325112867385, 1.000000000000000000, 0.9238795325112867385, 1.000000000000000000, 0.9238795325112867385, 1.000000000000000000, 0.9238795325112867385, 1.000000000000000000, 0.9238795325112867385, 1.000000000000000000, 0.9238795325112867385, 1.000000000000000000, 0.9238795325112867385, 1.000000000000000000, 0.9238795325112867385, 1.000000000000000000, 0.9238795325112867385, 1.000000000000000000, 0.9238795325112867385, 1.000000000000000000, 0.9238795325112867385, 1.000000000000000000, 0.9238795325112867385, 1.000000000000000000, 0.9238795325112867385, 1.000000000000000000, 0.9238795325112867385, 1.000000000000000000, 0.9238795325112867385, 1.000000000000000000, 0.9238795325112867385, 1.000000000000000000, 0.9238795325112867385, 1.000000000000000000, 0.9238795325112867385, 1.000000000000000000, 0.9238795325112867385, 1.000000000000000000, 0.9238795325112867385, 1.000000000000000000, 0.9238795325112867385, 1.000000000000000000, 0.9238795325112867385, 1.000000000000000000, 0.9238795325112867385, 1.000000000000000000, 0.9238795325112867385, 1.000000000000000000, 0.9238795325112867385, 1.000000000000000000, 0.9238795325112867385, 1.000000000000000000, 0.9238795325112867385, 1.000000000000000000, 0.9238795325112867385, 1.000000000000000000, 0.9238795325112867385, 1.000000000000000000, 0.9238795325112867385, 1.000000000000000000, 0.9238795325112867385, 1.000000000000000000, 0.9238795325112867385, 1.000000000000000000, 0.9238795325112867385, 1.000000000000000000, 0.9238795325112867385, 1.000000000000000000, 0.9238795325112867385, 1.000000000000000000, 0.9238795325112867385, 1.000000000000000000, 0.9238795325112867385, 1.000000000000000000, 0.9238795325112867385, 1.000000000000000000, 0.9238795325112867385, 1.000000000000000000, 0.9238795325112867385, 1.000000000000000000, 0.9238795325112867385, 1.000000000000000000, 0.9238795325112867385, 1.000000000000000000, 0.9238795325112867385, 1.000000000000000000, 0.9238795325112867385, 1.000000000000000000, 0.9238795325112867385, 1.000000000000000000, 0.9238795325112867385, 1.000000000000000000, 0.9238795325112867385, 1.000000000000000000, 0.9238795325112867385, 1.000000000000000000, 0.9238795325112867385, 1.000000000000000000, 0.9238795325112867385, 1.000000000000000000),
 ( 1.000000000000000000, 0.9238795325112867385, 1.000000000000000000, 0.9238795325112867385, 1.000000000000000000, 0.9238795325112867385, 1.000000000000000000, 0.9238795325112867385, 1.000000000000000000, 0.9238795325112867385, 1.000000000000000000, 0.9238795325112867385, 1.000000000000000000, 0.9238795325112867385, 1.000000000000000000, 0.9238795325112867385, 1.000000000000000000, 0.9238795325112867385, 1.000000000000000000, 0.9238795325112867385, 1.000000000000000000, 0.9238795325112867385, 1.000000000000000000, 0.9238795325112867385, 1.000000000000000000, 0.9238795325112867385, 1.000000000000000000, 0.9238795325112867385, 1.000000000000000000, 0.9238795325112867385, 1.000000000000000000, 0.9238795325112867385, 1.000000000000000000, 0.9238795325112867385, 1.000000000000000000, 0.9238795325112867385, 1.000000000000000000, 0.9238795325112867385, 1.000000000000000000, 0.9238795325112867385, 1.000000000000000000, 0.9238795325112867385, 1.000000000000000000, 0.9238795325112867385, 1.000000000000000000, 0.9238795325112867385, 1.000000000000000000, 0.9238795325112867385, 1.000000000000000000, 0.9238795325112867385, 1.000000000000000000, 0.9238795325112867385, 1.000000000000000000, 0.9238795325112867385, 1.000000000000000000, 0.9238795325112867385, 1.000000000000000000, 0.9238795325112867385, 1.000000000000000000, 0.9238795325112867385, 1.000000000000000000, 0.9238795325112867385, 1.000000000000000000, 0.9238795325112867385, 1.000000000000000000, 0.9238795325112867385, 1.000000000000000000, 0.9238795325112867385, 1.000000000000000000, 0.9238795325112867385, 1.000000000000000000, 0.9238795325112867385, 1.000000000000000000, 0.9238795325112867385, 1.000000000000000000, 0.9238795325112867385, 1.000000000000000000, 0.9238795325112867385, 1.000000000000000000, 0.9238795325112867385, 1.000000000000000000, 0.9238795325112867385, 1.000000000000000000, 0.9238795325112867385, 1.000000000000000000, 0.9238795325112867385, 1.000000000000000000, 0.9238795325112867385, 1.000000000000000000, 0.9238795325112867385, 1.000000000000000000, 0.9238795325112867385, 1.000000000000000000, 0.9238795325112867385, 1.000000000000000000, 0.9238795325112867385, 1.000000000000000000, 0.9238795325112867385, 1.000000000000000000, 0.9238795325112867385, 1.000000000000000000) ) ) 
 REPRESENTATION_ITEM ( '' )  SURFACE ( )  );
#4771 = VECTOR ( 'NONE', #11631, 1000.000000000000000 ) ;
#4772 = DIRECTION ( 'NONE',  ( 0.000000000000000000, 1.000000000000000000, 0.000000000000000000 ) ) ;
#4773 = CARTESIAN_POINT ( 'NONE',  ( -11.46040770435012668, -27.78091578003887463, 16.73242750791695954 ) ) ;
#4774 = CARTESIAN_POINT ( 'NONE',  ( -1.035533905932738863, 61.50000000000000000, 46.25000000218494733 ) ) ;
#4775 = CARTESIAN_POINT ( 'NONE',  ( -13.49542703274174116, -28.95583473709188738, 19.14257249208304401 ) ) ;
#4776 = CARTESIAN_POINT ( 'NONE',  ( -2.066987300000001415, 64.00000000000000000, 49.75000000109246656 ) ) ;
#4777 = CARTESIAN_POINT ( 'NONE',  ( -10.04416526290807710, -25.50457296725819489, 21.54492750791695599 ) ) ;
#4778 = DIRECTION ( 'NONE',  ( 1.000000000000000000, -0.000000000000000000, -0.000000000000000000 ) ) ;
#4779 = CARTESIAN_POINT ( 'NONE',  ( -11.21908421996108984, -20.46040770435011069, 15.41992750791695777 ) ) ;
#4780 = DIRECTION ( 'NONE',  ( 1.000000000000000000, 2.312964634635742957E-16, 0.000000000000000000 ) ) ;
#4781 = CARTESIAN_POINT ( 'NONE',  ( -44.99999999999998579, 3.000000000000000000, -55.00000000000000000 ) ) ;
#4782 = CARTESIAN_POINT ( 'NONE',  ( 2.066987300000001415, 64.00000000000000000, 46.95000000109246940 ) ) ;
#4783 = LINE ( 'NONE', #16227, #581 ) ;
#4784 = AXIS2_PLACEMENT_3D ( 'NONE', #12124, #4498, #18023 ) ;
#4785 = CARTESIAN_POINT ( 'NONE',  ( -19.99999999999999645, 0.000000000000000000, 1.500000000000000000 ) ) ;
#4786 = ADVANCED_FACE ( 'NONE', ( #10019 ), #5530, .T. ) ;
#4787 = CARTESIAN_POINT ( 'NONE',  ( 2.066987300000001415, 64.85617417291294373, 46.20000000109248361 ) ) ;
#4788 = CARTESIAN_POINT ( 'NONE',  ( 2.066987300000002303, 63.14382582708705627, 49.30000000109246372 ) ) ;
#4789 = DIRECTION ( 'NONE',  ( -1.000000000000000000, 0.000000000000000000, -0.000000000000000000 ) ) ;
#4790 = VERTEX_POINT ( 'NONE', #4459 ) ;
#4791 = EDGE_LOOP ( 'NONE', ( #3708, #3844, #17141, #5446, #1051 ) ) ;
#4792 = CARTESIAN_POINT ( 'NONE',  ( -20.24501739517669563, -18.99630608921239627, 31.83007249208304046 ) ) ;
#4793 =( LENGTH_UNIT ( ) NAMED_UNIT ( * ) SI_UNIT ( .MILLI., .METRE. ) );
#4794 = CARTESIAN_POINT ( 'NONE',  ( -17.64274437364858983, -19.75228648362910633, 16.29882249208304046 ) ) ;
#4795 = ORIENTED_EDGE ( 'NONE', *, *, #11894, .T. ) ;
#4796 = CARTESIAN_POINT ( 'NONE',  ( -12.04416526290807887, -24.96867458239596260, 16.29492750791696665 ) ) ;
#4797 = LINE ( 'NONE', #10746, #9252 ) ;
#4798 = CARTESIAN_POINT ( 'NONE',  ( -7.955834737091903364, -25.71081734191518464, 13.01757249208304046 ) ) ;
#4799 = CARTESIAN_POINT ( 'NONE',  ( -0.8561741729129465073, 61.93301270000000613, 48.90000000109247225 ) ) ;
#4800 = CARTESIAN_POINT ( 'NONE',  ( -0.8561741729129461742, 66.06698729999999387, 45.40000000109246514 ) ) ;
#4801 = ORIENTED_EDGE ( 'NONE', *, *, #1850, .T. ) ;
#4802 = ORIENTED_EDGE ( 'NONE', *, *, #13331, .T. ) ;
#4803 = CARTESIAN_POINT ( 'NONE',  ( -40.00000000000000711, 110.0000000000000000, -5.000000000000000888 ) ) ;
#4804 = FACE_OUTER_BOUND ( 'NONE', #13698, .T. ) ;
#4805 = ORIENTED_EDGE ( 'NONE', *, *, #13073, .T. ) ;
#4806 = CARTESIAN_POINT ( 'NONE',  ( -0.8561741729129466183, 61.93301270000000613, 48.10000000109246798 ) ) ;
#4807 = DIRECTION ( 'NONE',  ( 0.7071067811865414665, -0.5000000000000057732, 0.5000000000000028866 ) ) ;
#4808 = CARTESIAN_POINT ( 'NONE',  ( -2.066987300000001415, 63.14382582708705627, 45.80000000109246372 ) ) ;
#4809 = FACE_BOUND ( 'NONE', #1179, .T. ) ;
#4810 = CARTESIAN_POINT ( 'NONE',  ( -40.00000000000000711, 110.0000000000000000, -18.00000000000000000 ) ) ;
#4811 = ORIENTED_EDGE ( 'NONE', *, *, #12644, .T. ) ;
#4813 = ORIENTED_EDGE ( 'NONE', *, *, #2203, .F. ) ;
#4812 = ORIENTED_EDGE ( 'NONE', *, *, #569, .T. ) ;
#4814 = CARTESIAN_POINT ( 'NONE',  ( -8.044165262908075320, -26.04047135212042718, 16.29492750791696309 ) ) ;
#4815 = DIRECTION ( 'NONE',  ( 0.000000000000000000, 0.000000000000000000, 1.000000000000000000 ) ) ;
#4816 = ORIENTED_EDGE ( 'NONE', *, *, #5923, .F. ) ;
#4817 = ORIENTED_EDGE ( 'NONE', *, *, #11514, .T. ) ;
#4818 = CARTESIAN_POINT ( 'NONE',  ( -14.36097942780925685, -20.95583473709189093, 22.20507249208304401 ) ) ;
#4819 = CARTESIAN_POINT ( 'NONE',  ( -18.64274437364853654, -29.97976432393976509, 23.07617750791695954 ) ) ;
#4820 = CARTESIAN_POINT ( 'NONE',  ( -1.461580736456473906, 65.46158073645646880, 49.45000000109246940 ) ) ;
#4821 = DIRECTION ( 'NONE',  ( 1.000000000000000000, -0.000000000000000000, -0.000000000000000000 ) ) ;
#4822 = EDGE_LOOP ( 'NONE', ( #13936, #10362, #605, #12277 ) ) ;
#4823 = CARTESIAN_POINT ( 'NONE',  ( -15.16482700510260706, -26.99999999999998579, 12.13867750791695954 ) ) ;
#4824 = ORIENTED_EDGE ( 'NONE', *, *, #3381, .F. ) ;
#4825 = CARTESIAN_POINT ( 'NONE',  ( 1.035533905932739751, 61.50000000000000000, 45.44999999999999574 ) ) ;
#4826 = ORIENTED_EDGE ( 'NONE', *, *, #16711, .T. ) ;
#4827 = DIRECTION ( 'NONE',  ( -0.000000000000000000, 0.7071067811865497932, -0.7071067811865452413 ) ) ;
#4828 = CARTESIAN_POINT ( 'NONE',  ( 2.499999999999996447, 65.03553390593273775, 46.44999999999999574 ) ) ;
#4829 = PLANE ( 'NONE',  #4669 ) ;
#4830 = DIRECTION ( 'NONE',  ( -1.000000000000000000, -0.000000000000000000, 0.000000000000000000 ) ) ;
#4831 = CARTESIAN_POINT ( 'NONE',  ( -1.461580736456473462, 62.53841926354353120, 48.85000000109246798 ) ) ;
#4832 = CARTESIAN_POINT ( 'NONE',  ( -32.50000000000000000, 52.00000000000000711, 12.50000000000000000 ) ) ;
#4833 = CARTESIAN_POINT ( 'NONE',  ( -24.00000000000000711, 110.0000000000000000, -37.50000000000000711 ) ) ;
#4834 = CARTESIAN_POINT ( 'NONE',  ( 2.500000000000001776, 64.00000000000000000, 47.99999999999999289 ) ) ;
#4835 = LINE ( 'NONE', #1788, #10812 ) ;
#4836 = ORIENTED_EDGE ( 'NONE', *, *, #8898, .F. ) ;
#4837 = EDGE_CURVE ( 'NONE', #993, #7955, #17778, .T. ) ;
#4838 = CARTESIAN_POINT ( 'NONE',  ( -16.50457296725820555, -28.95583473709189448, 12.35742750791695954 ) ) ;
#4839 = CARTESIAN_POINT ( 'NONE',  ( 32.50000000000000000, 52.00000000000000711, 17.49999999999999645 ) ) ;
#4840 = ORIENTED_EDGE ( 'NONE', *, *, #13917, .F. ) ;
#4841 = CARTESIAN_POINT ( 'NONE',  ( -10.58745947852648328, -26.35725562635138530, 13.23632249208304046 ) ) ;
#4842 = CARTESIAN_POINT ( 'NONE',  ( -14.36097942780925685, -20.95583473709189093, 16.95507249208304046 ) ) ;
#4843 = ORIENTED_EDGE ( 'NONE', *, *, #13435, .T. ) ;
#4844 = DIRECTION ( 'NONE',  ( -0.000000000000000000, -1.000000000000000000, -0.000000000000000000 ) ) ;
#4845 = EDGE_LOOP ( 'NONE', ( #5703, #7004 ) ) ;
#4846 = CARTESIAN_POINT ( 'NONE',  ( 2.749999999999979128, 118.0000000000000142, -42.68883962248118991 ) ) ;
#4847 = CARTESIAN_POINT ( 'NONE',  ( -0.1250000000000104083, 27.16170093578836031, 58.97002704785691662 ) ) ;
#4848 = CARTESIAN_POINT ( 'NONE',  ( -40.00000000000000711, 113.0000000000000000, -6.000000000000005329 ) ) ;
#4849 = EDGE_CURVE ( 'NONE', #8051, #11742, #1410, .T. ) ;
#4850 = EDGE_CURVE ( 'NONE', #232, #13516, #19157, .T. ) ;
#4851 = AXIS2_PLACEMENT_3D ( 'NONE', #6420, #12582, #18576 ) ;
#4852 = DIRECTION ( 'NONE',  ( 0.000000000000000000, 0.7071067811865456854, 0.7071067811865494601 ) ) ;
#4853 = EDGE_CURVE ( 'NONE', #14478, #3100, #4356, .T. ) ;
#4854 = CARTESIAN_POINT ( 'NONE',  ( -32.50000000000000000, 47.00000000000000711, 12.50000000000000000 ) ) ;
#4855 = SURFACE_STYLE_USAGE ( .BOTH. , #12294 ) ;
#4856 = CARTESIAN_POINT ( 'NONE',  ( -0.9999999999999945599, -36.00000000000000711, 9.500000000000001776 ) ) ;
#4857 = VERTEX_POINT ( 'NONE', #4054 ) ;
#4859 = MECHANICAL_DESIGN_GEOMETRIC_PRESENTATION_REPRESENTATION (  '', ( #7343 ), #8585 ) ;
#4858 = DIRECTION ( 'NONE',  ( 0.000000000000000000, 0.000000000000000000, 1.000000000000000000 ) ) ;
#4860 = CARTESIAN_POINT ( 'NONE',  ( -15.16482700510259640, -28.99999999999998224, 12.13867750791695777 ) ) ;
#4861 = VECTOR ( 'NONE', #6043, 1000.000000000000000 ) ;
#4862 = CARTESIAN_POINT ( 'NONE',  ( 4.592425496802577917E-16, 61.50000000000000000, 46.30000000218493739 ) ) ;
#4863 = CARTESIAN_POINT ( 'NONE',  ( -16.17491895705296656, -29.04416526290807710, 19.58007249208303335 ) ) ;
#4864 = CARTESIAN_POINT ( 'NONE',  ( -2.283493650000001818, 64.00000000000000000, 49.87500000054622973 ) ) ;
#4865 = CARTESIAN_POINT ( 'NONE',  ( -10.04416526290807710, -25.50457296725819489, 11.04492750791695421 ) ) ;
#4866 = CARTESIAN_POINT ( 'NONE',  ( 2.500000000000001776, 64.00000000000000000, 48.10000000218494165 ) ) ;
#4867 = CARTESIAN_POINT ( 'NONE',  ( -19.41254052147348830, -26.35725562635142083, 18.26367750791695599 ) ) ;
#4868 = PLANE ( 'NONE',  #15624 ) ;
#4869 = LINE ( 'NONE', #8805, #11952 ) ;
#4870 = ADVANCED_FACE ( 'NONE', ( #6994 ), #16110, .F. ) ;
#4871 = CARTESIAN_POINT ( 'NONE',  ( 1.461580736456473906, 62.53841926354353120, 47.65000000109247225 ) ) ;
#4872 = FACE_OUTER_BOUND ( 'NONE', #11358, .T. ) ;
#4873 = AXIS2_PLACEMENT_3D ( 'NONE', #18192, #4772, #15047 ) ;
#4874 = CARTESIAN_POINT ( 'NONE',  ( 0.000000000000000000, 64.00000000000000000, 49.99999999999999289 ) ) ;
#4875 = VECTOR ( 'NONE', #8062, 1000.000000000000000 ) ;
#4876 = CARTESIAN_POINT ( 'NONE',  ( 0.8561741729129472844, 61.93301270000000613, 46.80000000109246372 ) ) ;
#4877 = CARTESIAN_POINT ( 'NONE',  ( 2.500000000000000000, -2.357898499370432610, 3.252606517456513302E-15 ) ) ;
#4878 = ORIENTED_EDGE ( 'NONE', *, *, #13459, .F. ) ;
#4879 = ORIENTED_EDGE ( 'NONE', *, *, #6769, .T. ) ;
#4880 = CARTESIAN_POINT ( 'NONE',  ( -21.95583473709189803, -26.04047135212049469, 30.95507249208304401 ) ) ;
#4881 =( NAMED_UNIT ( * ) PLANE_ANGLE_UNIT ( ) SI_UNIT ( $, .RADIAN. ) );
#4882 = CARTESIAN_POINT ( 'NONE',  ( -11.21908421996106142, -27.53959229564982181, 8.205072492083040459 ) ) ;
#4883 = EDGE_LOOP ( 'NONE', ( #1540, #2610, #3452, #10657 ) ) ;
#4884 = CARTESIAN_POINT ( 'NONE',  ( -17.99999999999999645, -23.83517299489736985, 29.20117750791695954 ) ) ;
#4885 = DIRECTION ( 'NONE',  ( 0.000000000000000000, 0.000000000000000000, -1.000000000000000000 ) ) ;
#4886 = CARTESIAN_POINT ( 'NONE',  ( -8.855408670957602979, -27.35725562635137820, 13.23632249208303868 ) ) ;
#4887 = VECTOR ( 'NONE', #3550, 1000.000000000000114 ) ;
#4888 = AXIS2_PLACEMENT_3D ( 'NONE', #7728, #3216, #15176 ) ;
#4889 = CARTESIAN_POINT ( 'NONE',  ( 2.066987300000001415, 64.00000000000000000, 45.15000000109247225 ) ) ;
#4890 = CARTESIAN_POINT ( 'NONE',  ( 2.066987300000002303, 63.14382582708705627, 45.10000000109246798 ) ) ;
#4891 = ORIENTED_EDGE ( 'NONE', *, *, #1564, .F. ) ;
#4892 = EDGE_CURVE ( 'NONE', #6563, #9100, #14539, .T. ) ;
#4893 = ORIENTED_EDGE ( 'NONE', *, *, #2433, .T. ) ;
#4894 = CARTESIAN_POINT ( 'NONE',  ( 43.49999999999997868, 115.0000000000000000, -52.50000000000002132 ) ) ;
#4895 = CARTESIAN_POINT ( 'NONE',  ( 0.1499999999999973577, 0.000000000000000000, 2.750000000000000000 ) ) ;
#4896 = VERTEX_POINT ( 'NONE', #13056 ) ;
#4897 = CARTESIAN_POINT ( 'NONE',  ( 1.461580736456473906, 62.53841926354353120, 49.05000000109247082 ) ) ;
#4898 = CARTESIAN_POINT ( 'NONE',  ( -2.492551403682614186, 28.10514068711927749, 58.38014068711927251 ) ) ;
#4899 = CARTESIAN_POINT ( 'NONE',  ( 1.300000000000000044, 1.478016689125442484, -1.626303258728256651E-15 ) ) ;
#4900 = EDGE_CURVE ( 'NONE', #3619, #16545, #13141, .T. ) ;
#4901 = LINE ( 'NONE', #17048, #12567 ) ;
#4902 = VECTOR ( 'NONE', #1143, 1000.000000000000000 ) ;
#4903 = VECTOR ( 'NONE', #8861, 1000.000000000000000 ) ;
#4904 = CARTESIAN_POINT ( 'NONE',  ( 1.767766952966370653, 62.23223304703363112, 45.60000000218494165 ) ) ;
#4905 = ORIENTED_EDGE ( 'NONE', *, *, #7714, .T. ) ;
#4907 = EDGE_LOOP ( 'NONE', ( #2823, #14575, #18369, #4127, #15491 ) ) ;
#4906 = ORIENTED_EDGE ( 'NONE', *, *, #9838, .F. ) ;
#4908 = CARTESIAN_POINT ( 'NONE',  ( -7.955834737091916686, -22.28918265808470522, 26.35742750791695954 ) ) ;
#4909 = ORIENTED_EDGE ( 'NONE', *, *, #14060, .T. ) ;
#4910 = ORIENTED_EDGE ( 'NONE', *, *, #15426, .T. ) ;
#4911 = CARTESIAN_POINT ( 'NONE',  ( -16.64274437364858272, -21.48433729119797420, 21.54882249208304401 ) ) ;
#4912 = CARTESIAN_POINT ( 'NONE',  ( -20.24501739517664234, -29.00369391078761439, 18.04492750791695954 ) ) ;
#4913 = CARTESIAN_POINT ( 'NONE',  ( -2.066987300000001415, 64.00000000000000000, 47.15000000109247225 ) ) ;
#4914 = LINE ( 'NONE', #9404, #15959 ) ;
#4915 = EDGE_CURVE ( 'NONE', #14031, #10014, #8978, .T. ) ;
#4916 = VERTEX_POINT ( 'NONE', #16206 ) ;
#4917 = CARTESIAN_POINT ( 'NONE',  ( -12.48433729119798130, -25.64274437364855075, 11.26367750791696132 ) ) ;
#4918 = AXIS2_PLACEMENT_3D ( 'NONE', #7468, #10200, #18068 ) ;
#4919 = FILL_AREA_STYLE ('',( #18254 ) ) ;
#4920 = ORIENTED_EDGE ( 'NONE', *, *, #9760, .F. ) ;
#4921 = CIRCLE ( 'NONE', #8348, 10.00000000000000178 ) ;
#4922 = DIRECTION ( 'NONE',  ( -0.000000000000000000, 1.000000000000000000, 0.000000000000000000 ) ) ;
#4923 = ORIENTED_EDGE ( 'NONE', *, *, #4509, .F. ) ;
#4924 = CARTESIAN_POINT ( 'NONE',  ( -50.00000000000001421, 3.000000000000000000, 59.99999999999997868 ) ) ;
#4925 = DIRECTION ( 'NONE',  ( -0.000000000000000000, 0.7071067811865493491, -0.7071067811865456854 ) ) ;
#4926 = CARTESIAN_POINT ( 'NONE',  ( -15.00000000000000000, 0.000000000000000000, 7.999999999999996447 ) ) ;
#4927 = DIRECTION ( 'NONE',  ( -0.000000000000000000, -1.000000000000000000, -0.000000000000000000 ) ) ;
#4928 = CARTESIAN_POINT ( 'NONE',  ( -0.8561741729129465073, 61.93301270000000613, 48.90000000109247225 ) ) ;
#4929 = ITEM_DEFINED_TRANSFORMATION ( 'NONE', 'NONE', #4545,  #1791 ) ;
#4930 = CARTESIAN_POINT ( 'NONE',  ( 1.035533905932738197, 66.50000000000000000, 49.05000000218495160 ) ) ;
#4931 = FACE_OUTER_BOUND ( 'NONE', #1062, .T. ) ;
#4932 = CARTESIAN_POINT ( 'NONE',  ( -41.00000000000000711, 53.00000000000000711, -5.000000000000000888 ) ) ;
#4933 = CARTESIAN_POINT ( 'NONE',  ( -2.066987300000001415, 64.00000000000000000, 49.75000000109246656 ) ) ;
#4934 = ORIENTED_EDGE ( 'NONE', *, *, #4208, .F. ) ;
#4935 = CARTESIAN_POINT ( 'NONE',  ( -13.49542703274178379, -19.04416526290806289, 35.98242750791696665 ) ) ;
#4936 = CIRCLE ( 'NONE', #3973, 1.500000000000001332 ) ;
#4937 = DIRECTION ( 'NONE',  ( 1.000000000000000000, 0.000000000000000000, 0.000000000000000000 ) ) ;
#4938 = ORIENTED_EDGE ( 'NONE', *, *, #9001, .T. ) ;
#4939 = UNCERTAINTY_MEASURE_WITH_UNIT (LENGTH_MEASURE( 1.000000000000000082E-05 ), #17400, 'distance_accuracy_value', 'NONE');
#4940 = CARTESIAN_POINT ( 'NONE',  ( -13.49542703274174116, -28.95583473709188738, 19.14257249208304401 ) ) ;
#4941 = CARTESIAN_POINT ( 'NONE',  ( -16.64274437364858272, -21.48433729119797420, 21.54882249208304401 ) ) ;
#4942 = CARTESIAN_POINT ( 'NONE',  ( -3.065533689247737392, -45.28611686177728046, 3.000000000000000000 ) ) ;
#4943 = VERTEX_POINT ( 'NONE', #2773 ) ;
#4944 = LINE ( 'NONE', #17091, #7502 ) ;
#4945 = VERTEX_POINT ( 'NONE', #8750 ) ;
#4946 = CARTESIAN_POINT ( 'NONE',  ( -2.066987300000001415, 64.00000000000000000, 49.65000000109247225 ) ) ;
#4947 = EDGE_CURVE ( 'NONE', #18471, #2469, #2740, .T. ) ;
#4948 = ADVANCED_FACE ( 'NONE', ( #16780, #8150 ), #7960, .T. ) ;
#4949 = FACE_BOUND ( 'NONE', #8943, .T. ) ;
#4950 = FACE_OUTER_BOUND ( 'NONE', #13209, .T. ) ;
#4951 = CARTESIAN_POINT ( 'NONE',  ( -2.066987300000001415, 64.85617417291294373, 44.90000000109247225 ) ) ;
#4952 = ADVANCED_FACE ( 'NONE', ( #16877 ), #6680, .F. ) ;
#4953 = LINE ( 'NONE', #15436, #15475 ) ;
#4954 = PRESENTATION_STYLE_ASSIGNMENT (( #4855 ) ) ;
#4956 = ADVANCED_FACE ( 'NONE', ( #7865 ), #2069, .T. ) ;
#4955 = DIRECTION ( 'NONE',  ( -0.000000000000000000, 1.000000000000000000, -0.000000000000000000 ) ) ;
#4957 = EDGE_LOOP ( 'NONE', ( #16348, #15769, #18237, #5779 ) ) ;
#4958 = CARTESIAN_POINT ( 'NONE',  ( -16.17491895705301275, -18.95583473709189803, 19.79492750791695954 ) ) ;
#4959 = CARTESIAN_POINT ( 'NONE',  ( 1.767766952966370653, 62.23223304703363112, 46.40000000218494591 ) ) ;
#4960 = EDGE_CURVE ( 'NONE', #9953, #11135, #3353, .T. ) ;
#4961 = CARTESIAN_POINT ( 'NONE',  ( -19.41254052147350961, -21.64274437364857562, 21.11132249208304401 ) ) ;
#4962 = DIRECTION ( 'NONE',  ( -0.8660254037844385966, 0.000000000000000000, 0.5000000000000001110 ) ) ;
#4963 = CARTESIAN_POINT ( 'NONE',  ( -11.46040770435012668, -27.78091578003887463, 11.48242750791695954 ) ) ;
#4964 = CARTESIAN_POINT ( 'NONE',  ( -24.00000000000000000, 52.00000000000000711, 18.00000000000000000 ) ) ;
#4965 = CARTESIAN_POINT ( 'NONE',  ( -13.82508104294698015, -29.04416526290806289, 17.16992750791695244 ) ) ;
#4966 = CARTESIAN_POINT ( 'NONE',  ( -19.95583473709190514, -25.50457296725823042, 25.70507249208304756 ) ) ;
#4967 = EDGE_CURVE ( 'NONE', #15935, #17810, #11074, .T. ) ;
#4968 = CARTESIAN_POINT ( 'NONE',  ( -1.265664690411616068E-16, 66.06698730000000808, 47.95000000109246940 ) ) ;
#4969 = CARTESIAN_POINT ( 'NONE',  ( 2.500000000000001776, 64.00000000000000000, 49.60000000000000142 ) ) ;
#4970 = DIRECTION ( 'NONE',  ( -1.000000000000000000, -0.000000000000000000, -0.000000000000000000 ) ) ;
#4971 = CARTESIAN_POINT ( 'NONE',  ( -1.767766952966370209, 65.76776695296638309, 48.40000000218494591 ) ) ;
#4972 = CARTESIAN_POINT ( 'NONE',  ( 1.461580736456473684, 65.46158073645646880, 48.65000000109247225 ) ) ;
#4973 = CARTESIAN_POINT ( 'NONE',  ( -32.50000000000000000, 52.00000000000000711, 15.00000000000000000 ) ) ;
#4974 = AXIS2_PLACEMENT_3D ( 'NONE', #16134, #11418, #8305 ) ;
#4975 = ORIENTED_EDGE ( 'NONE', *, *, #15493, .T. ) ;
#4976 = ORIENTED_EDGE ( 'NONE', *, *, #3157, .T. ) ;
#4977 = CARTESIAN_POINT ( 'NONE',  ( -8.855408670957602979, -27.35725562635137820, 34.23632249208304046 ) ) ;
#4978 = EDGE_CURVE ( 'NONE', #8057, #16018, #408, .T. ) ;
#4979 = CARTESIAN_POINT ( 'NONE',  ( -10.58745947852648328, -26.35725562635138530, 13.23632249208304046 ) ) ;
#4981 = VERTEX_POINT ( 'NONE', #13832 ) ;
#4980 = EDGE_CURVE ( 'NONE', #3066, #10268, #594, .T. ) ;
#4982 = CARTESIAN_POINT ( 'NONE',  ( -15.63902057219076269, -20.95583473709189448, 25.04492750791696309 ) ) ;
#4983 = CARTESIAN_POINT ( 'NONE',  ( -15.00000000000000000, 35.00000000000000000, 37.00000000000000000 ) ) ;
#4984 = CARTESIAN_POINT ( 'NONE',  ( -18.64274437364860049, -18.02023567606023491, 16.29882249208303691 ) ) ;
#4985 = CARTESIAN_POINT ( 'NONE',  ( 2.066987300000002303, 63.14382582708705627, 45.10000000109246798 ) ) ;
#4986 = CARTESIAN_POINT ( 'NONE',  ( 0.8561741729129472844, 61.93301270000000613, 45.00000000109246656 ) ) ;
#4987 = ORIENTED_EDGE ( 'NONE', *, *, #6720, .T. ) ;
#4988 = ORIENTED_EDGE ( 'NONE', *, *, #9738, .F. ) ;
#4989 = EDGE_CURVE ( 'NONE', #8458, #14577, #2163, .T. ) ;
#4990 = AXIS2_PLACEMENT_3D ( 'NONE', #13555, #10412, #1411 ) ;
#4991 = CARTESIAN_POINT ( 'NONE',  ( -10.00000000000000000, -32.50000000000000711, 1.500000000000000444 ) ) ;
#4992 = LINE ( 'NONE', #16951, #4470 ) ;
#4993 = CARTESIAN_POINT ( 'NONE',  ( -1.265664690411616068E-16, 66.06698730000000808, 49.35000000109246798 ) ) ;
#4994 = DIRECTION ( 'NONE',  ( -0.000000000000000000, -0.000000000000000000, -1.000000000000000000 ) ) ;
#4995 = DIRECTION ( 'NONE',  ( 0.000000000000000000, 0.000000000000000000, 1.000000000000000000 ) ) ;
#4996 = CYLINDRICAL_SURFACE ( 'NONE', #9726, 10.00000000000000000 ) ;
#4997 = VECTOR ( 'NONE', #14685, 1000.000000000000114 ) ;
#4998 = CARTESIAN_POINT ( 'NONE',  ( -40.00000000000000711, 110.0000000000000000, -5.999999999999998224 ) ) ;
#4999 = EDGE_CURVE ( 'NONE', #3996, #16018, #18552, .T. ) ;
#5000 = ORIENTED_EDGE ( 'NONE', *, *, #9256, .F. ) ;
#5001 = ORIENTED_EDGE ( 'NONE', *, *, #756, .F. ) ;
#5002 = CARTESIAN_POINT ( 'NONE',  ( -8.044165262908075320, -26.04047135212042718, 37.29492750791695954 ) ) ;
#5003 = ORIENTED_EDGE ( 'NONE', *, *, #4457, .T. ) ;
#5004 = VECTOR ( 'NONE', #91, 1000.000000000000114 ) ;
#5005 = ORIENTED_EDGE ( 'NONE', *, *, #6984, .T. ) ;
#5006 = CARTESIAN_POINT ( 'NONE',  ( -14.83517299489736985, -26.99999999999998579, 29.86132249208304756 ) ) ;
#5007 = CARTESIAN_POINT ( 'NONE',  ( -13.28918265808472299, -31.04416526290805933, 22.41992750791695954 ) ) ;
#5008 = CARTESIAN_POINT ( 'NONE',  ( -0.8561741729129466183, 61.93301270000000613, 48.90000000109247225 ) ) ;
#5009 = CARTESIAN_POINT ( 'NONE',  ( -40.00000000000000711, 110.0000000000000000, 27.50000000000000000 ) ) ;
#5010 = VERTEX_POINT ( 'NONE', #18260 ) ;
#5011 = CARTESIAN_POINT ( 'NONE',  ( -12.04416526290807887, -24.96867458239596260, 37.29492750791695954 ) ) ;
#5012 = VECTOR ( 'NONE', #9716, 1000.000000000000000 ) ;
#5013 = DIRECTION ( 'NONE',  ( -5.782411586589357392E-17, 0.000000000000000000, -1.000000000000000000 ) ) ;
#5014 = ORIENTED_EDGE ( 'NONE', *, *, #15260, .T. ) ;
#5015 = DIRECTION ( 'NONE',  ( 0.000000000000000000, -0.7071067811865457964, -0.7071067811865492381 ) ) ;
#5016 = ORIENTED_EDGE ( 'NONE', *, *, #2860, .F. ) ;
#5017 = LINE ( 'NONE', #972, #14753 ) ;
#5018 = DIRECTION ( 'NONE',  ( 0.000000000000000000, 0.000000000000000000, -1.000000000000000000 ) ) ;
#5019 = FACE_OUTER_BOUND ( 'NONE', #1144, .T. ) ;
#5020 = FACE_BOUND ( 'NONE', #1059, .T. ) ;
#5021 = VECTOR ( 'NONE', #8372, 1000.000000000000000 ) ;
#5022 = CARTESIAN_POINT ( 'NONE',  ( 2.066987300000001415, 64.00000000000000000, 48.35000000109246798 ) ) ;
#5023 = DIRECTION ( 'NONE',  ( 1.110223024625156540E-16, 0.7071067811865455743, 0.7071067811865494601 ) ) ;
#5024 = DIRECTION ( 'NONE',  ( 0.000000000000000000, 0.000000000000000000, 1.000000000000000000 ) ) ;
#5025 = CARTESIAN_POINT ( 'NONE',  ( 2.500000000000001776, 64.00000000000000000, 49.60000000000000142 ) ) ;
#5026 = AXIS2_PLACEMENT_3D ( 'NONE', #3532, #584, #8050 ) ;
#5027 = FACE_OUTER_BOUND ( 'NONE', #4489, .T. ) ;
#5028 = EDGE_LOOP ( 'NONE', ( #6303, #9952, #16859, #4251 ) ) ;
#5029 = CARTESIAN_POINT ( 'NONE',  ( -9.999999999999994671, -24.16482700510257686, 31.82617750791696309 ) ) ;
#5030 = CARTESIAN_POINT ( 'NONE',  ( 24.00000000000000000, 52.00000000000000711, 18.00000000000000355 ) ) ;
#5031 = ORIENTED_EDGE ( 'NONE', *, *, #11769, .T. ) ;
#5032 = VECTOR ( 'NONE', #14942, 1000.000000000000000 ) ;
#5033 = CARTESIAN_POINT ( 'NONE',  ( -18.78091578003892081, -20.46040770435013556, 37.08007249208304046 ) ) ;
#5034 = AXIS2_PLACEMENT_3D ( 'NONE', #2158, #2346, #14303 ) ;
#5035 = CARTESIAN_POINT ( 'NONE',  ( -16.64274437364858272, -21.48433729119797420, 16.29882249208304401 ) ) ;
#5036 = CARTESIAN_POINT ( 'NONE',  ( -24.00000000000000000, 110.0000000000000000, 30.00000000000000000 ) ) ;
#5037 = ORIENTED_EDGE ( 'NONE', *, *, #3847, .T. ) ;
#5038 = DIRECTION ( 'NONE',  ( -0.000000000000000000, 1.000000000000000000, 0.000000000000000000 ) ) ;
#5039 = ORIENTED_EDGE ( 'NONE', *, *, #9036, .T. ) ;
#5040 = DIRECTION ( 'NONE',  ( 0.000000000000000000, 1.000000000000000000, 0.000000000000000000 ) ) ;
#5041 = CARTESIAN_POINT ( 'NONE',  ( -41.00000000000000711, 53.00000000000000711, 14.50000000000000000 ) ) ;
#5042 = DIRECTION ( 'NONE',  ( 1.000000000000000000, 0.000000000000000000, 0.000000000000000000 ) ) ;
#5043 = VECTOR ( 'NONE', #13923, 1000.000000000000000 ) ;
#5044 = LINE ( 'NONE', #7892, #8451 ) ;
#5045 = LINE ( 'NONE', #16712, #9211 ) ;
#5046 = DIRECTION ( 'NONE',  ( 1.000000000000000000, 0.000000000000000000, 0.000000000000000000 ) ) ;
#5047 = DIRECTION ( 'NONE',  ( 0.000000000000000000, 0.000000000000000000, -1.000000000000000000 ) ) ;
#5048 = CARTESIAN_POINT ( 'NONE',  ( 2.500000000000000000, 1.178949249685212974, -2.042000000000001148 ) ) ;
#5049 = VECTOR ( 'NONE', #8, 1000.000000000000000 ) ;
#5050 = ADVANCED_FACE ( 'NONE', ( #13924 ), #4829, .T. ) ;
#5051 = EDGE_LOOP ( 'NONE', ( #881, #11264, #6472, #779 ) ) ;
#5052 = EDGE_CURVE ( 'NONE', #17270, #9938, #13728, .T. ) ;
#5053 = AXIS2_PLACEMENT_3D ( 'NONE', #11050, #17047, #9200 ) ;
#5054 = CARTESIAN_POINT ( 'NONE',  ( -12.35725562635143682, -19.75228648362908501, 15.20117750791695777 ) ) ;
#5055 = CARTESIAN_POINT ( 'NONE',  ( 2.500000000000001776, 64.00000000000000000, 45.70000000218494307 ) ) ;
#5056 = ADVANCED_FACE ( 'NONE', ( #16982 ), #1879, .T. ) ;
#5057 = CARTESIAN_POINT ( 'NONE',  ( -20.04416526290809131, -22.82508104294699791, 15.64257249208304223 ) ) ;
#5058 = VECTOR ( 'NONE', #17914, 1000.000000000000000 ) ;
#5059 = PLANE ( 'NONE',  #18864 ) ;
#5060 = CARTESIAN_POINT ( 'NONE',  ( -14.83517299489739649, -18.99999999999997868, 14.76367750791695777 ) ) ;
#5061 = EDGE_CURVE ( 'NONE', #6083, #9185, #6487, .T. ) ;
#5062 = CLOSED_SHELL ( 'NONE', ( #2260, #1064, #5346, #15951, #8191, #418, #9634, #13208, #7215, #4582, #9004, #6522, #13750, #17485, #11180, #5784, #14930, #3197, #6379, #4952, #8175, #7414, #8034, #18742, #18530, #9725, #5556 ) ) ;
#5063 = CARTESIAN_POINT ( 'NONE',  ( 32.50000000000000000, 52.00000000000000711, -32.50000000000000000 ) ) ;
#5064 = CARTESIAN_POINT ( 'NONE',  ( -19.99999999999999645, -23.83517299489738051, 29.20117750791695599 ) ) ;
#5065 = DIRECTION ( 'NONE',  ( -1.000000000000000000, 0.000000000000000000, 0.000000000000000000 ) ) ;
#5066 = CARTESIAN_POINT ( 'NONE',  ( -18.53959229564983247, -27.78091578003891016, 30.51757249208304401 ) ) ;
#5067 = CARTESIAN_POINT ( 'NONE',  ( -1.461580736456473906, 65.46158073645646880, 48.05000000109247082 ) ) ;
#5068 = FACE_OUTER_BOUND ( 'NONE', #10560, .T. ) ;
#5069 = CARTESIAN_POINT ( 'NONE',  ( -24.00000000000000711, 110.0000000000000000, -11.50000000000000000 ) ) ;
#5070 = VECTOR ( 'NONE', #14961, 1000.000000000000000 ) ;
#5071 = SURFACE_SIDE_STYLE ('',( #549 ) ) ;
#5072 = CARTESIAN_POINT ( 'NONE',  ( -0.8561741729129465073, 61.93301270000000613, 49.10000000109246088 ) ) ;
#5073 = CARTESIAN_POINT ( 'NONE',  ( -4.000000000000001776, 67.00000000000000000, 34.99999999999999289 ) ) ;
#5074 = ORIENTED_EDGE ( 'NONE', *, *, #5719, .T. ) ;
#5075 = ORIENTED_EDGE ( 'NONE', *, *, #14964, .F. ) ;
#5076 = CARTESIAN_POINT ( 'NONE',  ( -21.99999999999999289, -24.16482700510262305, 36.42382249208304756 ) ) ;
#5077 = EDGE_CURVE ( 'NONE', #5207, #16010, #4067, .T. ) ;
#5078 = CARTESIAN_POINT ( 'NONE',  ( -13.82508104294702100, -18.95583473709188382, 16.95507249208304401 ) ) ;
#5079 = VERTEX_POINT ( 'NONE', #10977 ) ;
#5080 = CARTESIAN_POINT ( 'NONE',  ( -12.48433729119798130, -25.64274437364855075, 32.26367750791695954 ) ) ;
#5081 = APPLICATION_CONTEXT ( 'automotive_design' ) ;
#5082 = DIRECTION ( 'NONE',  ( -1.000000000000000000, 0.000000000000000000, -0.000000000000000000 ) ) ;
#5083 = CARTESIAN_POINT ( 'NONE',  ( -12.95952864787948755, -30.95583473709188382, 13.89257249208304046 ) ) ;
#5084 = AXIS2_PLACEMENT_3D ( 'NONE', #6005, #13634, #11967 ) ;
#5085 = CARTESIAN_POINT ( 'NONE',  ( 2.066987300000001415, 64.00000000000000000, 46.75000000109247367 ) ) ;
#5086 = CARTESIAN_POINT ( 'NONE',  ( 1.767766952966370653, 62.23223304703363112, 48.69999999999999574 ) ) ;
#5087 = ORIENTED_EDGE ( 'NONE', *, *, #14302, .F. ) ;
#5088 = ORIENTED_EDGE ( 'NONE', *, *, #1876, .F. ) ;
#5089 = AXIS2_PLACEMENT_3D ( 'NONE', #17314, #3877, #17492 ) ;
#5090 = DIRECTION ( 'NONE',  ( 0.000000000000000000, 0.000000000000000000, 1.000000000000000000 ) ) ;
#5091 = LINE ( 'NONE', #10855, #17006 ) ;
#5092 = CARTESIAN_POINT ( 'NONE',  ( 4.012830983233651061, 32.52836399182262994, 53.60336399182268252 ) ) ;
#5093 = DIRECTION ( 'NONE',  ( -0.000000000000000000, -0.000000000000000000, -1.000000000000000000 ) ) ;
#5094 = CYLINDRICAL_SURFACE ( 'NONE', #5053, 2.500000000000001776 ) ;
#5095 = ADVANCED_FACE ( 'NONE', ( #3541, #3634, #9510, #8059, #14020, #18915, #11253 ), #873, .T. ) ;
#5096 = ADVANCED_FACE ( 'NONE', ( #4008 ), #3824, .T. ) ;
#5097 = LINE ( 'NONE', #3416, #12235 ) ;
#5098 = ADVANCED_FACE ( 'NONE', ( #2437 ), #5577, .T. ) ;
#5099 = DIRECTION ( 'NONE',  ( 0.000000000000000000, 0.000000000000000000, -1.000000000000000000 ) ) ;
#5100 = ORIENTED_EDGE ( 'NONE', *, *, #13421, .T. ) ;
#5101 = ORIENTED_EDGE ( 'NONE', *, *, #11513, .T. ) ;
#5102 = CARTESIAN_POINT ( 'NONE',  ( -20.24501739517664234, -29.00369391078761439, 28.54492750791695954 ) ) ;
#5103 = ORIENTED_EDGE ( 'NONE', *, *, #5061, .F. ) ;
#5105 = EDGE_LOOP ( 'NONE', ( #5985, #18335, #3220, #12115 ) ) ;
#5104 = VERTEX_POINT ( 'NONE', #8248 ) ;
#5106 = CARTESIAN_POINT ( 'NONE',  ( -15.96867458239599635, -21.04416526290806999, 32.26757249208305467 ) ) ;
#5107 = CARTESIAN_POINT ( 'NONE',  ( -21.95583473709191580, -21.95952864787954084, 24.16992750791695954 ) ) ;
#5108 = VECTOR ( 'NONE', #1752, 1000.000000000000000 ) ;
#5109 = DIRECTION ( 'NONE',  ( -0.000000000000000000, -1.000000000000000000, -0.000000000000000000 ) ) ;
#5110 = CARTESIAN_POINT ( 'NONE',  ( 0.8561741729129471734, 61.93301270000000613, 48.20000000109247651 ) ) ;
#5111 = DIRECTION ( 'NONE',  ( 0.000000000000000000, 0.000000000000000000, 1.000000000000000000 ) ) ;
#5112 = ORIENTED_EDGE ( 'NONE', *, *, #12038, .F. ) ;
#5113 = CARTESIAN_POINT ( 'NONE',  ( -17.31681416490115311, -26.07549068051209318, 28.54492750791696665 ) ) ;
#5114 = CARTESIAN_POINT ( 'NONE',  ( -24.00000000000000000, 0.000000000000000000, 18.00000000000000355 ) ) ;
#5115 = ORIENTED_EDGE ( 'NONE', *, *, #13054, .T. ) ;
#5116 = CARTESIAN_POINT ( 'NONE',  ( -24.00000000000000711, 53.00000000000000711, 27.50000000000000000 ) ) ;
#5117 = ORIENTED_EDGE ( 'NONE', *, *, #9278, .F. ) ;
#5118 = PLANE ( 'NONE',  #13506 ) ;
#5119 = ADVANCED_FACE ( 'NONE', ( #15971, #11444 ), #13011, .T. ) ;
#5120 = ADVANCED_FACE ( 'NONE', ( #18822 ), #5396, .T. ) ;
#5121 = CARTESIAN_POINT ( 'NONE',  ( -41.00000000000000711, 110.0000000000000000, 8.000000000000000000 ) ) ;
#5122 = FACE_OUTER_BOUND ( 'NONE', #13588, .T. ) ;
#5123 = FACE_BOUND ( 'NONE', #11926, .T. ) ;
#5124 = CARTESIAN_POINT ( 'NONE',  ( 2.066987300000002303, 63.14382582708705627, 48.30000000109247082 ) ) ;
#5125 = ITEM_DEFINED_TRANSFORMATION ( 'NONE', 'NONE', #2652,  #1791 ) ;
#5126 = CARTESIAN_POINT ( 'NONE',  ( 3.796994071234847710E-16, 61.93301269999999903, 49.15000000109246514 ) ) ;
#5127 = CARTESIAN_POINT ( 'NONE',  ( -41.00000000000000711, 110.0000000000000000, -38.50000000000000711 ) ) ;
#5128 = LINE ( 'NONE', #11081, #15557 ) ;
#5129 = CARTESIAN_POINT ( 'NONE',  ( 2.227674122569385240, 64.95406575718618569, 45.00000000000000711 ) ) ;
#5130 = ORIENTED_EDGE ( 'NONE', *, *, #15022, .T. ) ;
#5131 = CARTESIAN_POINT ( 'NONE',  ( -12.35725562635143682, -19.75228648362908501, 25.70117750791695599 ) ) ;
#5132 = DIRECTION ( 'NONE',  ( -1.541976423090495880E-16, 0.000000000000000000, 1.000000000000000000 ) ) ;
#5133 = ORIENTED_EDGE ( 'NONE', *, *, #6964, .F. ) ;
#5134 = CARTESIAN_POINT ( 'NONE',  ( -9.955834737091903364, -25.17491895705294880, 28.76757249208304401 ) ) ;
#5135 = CARTESIAN_POINT ( 'NONE',  ( -12.04416526290808420, -23.03132541760398766, 28.33007249208304756 ) ) ;
#5136 = ORIENTED_EDGE ( 'NONE', *, *, #436, .F. ) ;
#5137 = DIRECTION ( 'NONE',  ( 0.000000000000000000, -1.224646799147353454E-16, 1.000000000000000000 ) ) ;
#5138 = ORIENTED_EDGE ( 'NONE', *, *, #17086, .F. ) ;
#5139 = EDGE_CURVE ( 'NONE', #10078, #16767, #2535, .T. ) ;
#5140 = CYLINDRICAL_SURFACE ( 'NONE', #17219, 1.678500596222258556 ) ;
#5141 = FACE_OUTER_BOUND ( 'NONE', #2421, .T. ) ;
#5142 = LINE ( 'NONE', #8082, #14129 ) ;
#5143 = DIRECTION ( 'NONE',  ( 0.000000000000000000, -0.000000000000000000, 1.000000000000000000 ) ) ;
#5144 = CARTESIAN_POINT ( 'NONE',  ( 2.500000000000000000, 2.357898499370431722, -2.818925648462311528E-15 ) ) ;
#5145 = UNCERTAINTY_MEASURE_WITH_UNIT (LENGTH_MEASURE( 1.000000000000000082E-05 ), #3280, 'distance_accuracy_value', 'NONE');
#5146 = ORIENTED_EDGE ( 'NONE', *, *, #10597, .F. ) ;
#5147 = CARTESIAN_POINT ( 'NONE',  ( -12.64274437364855252, -28.41254052147347053, 27.45117750791695954 ) ) ;
#5148 = CARTESIAN_POINT ( 'NONE',  ( -1.767766952966369765, 62.23223304703363112, 45.40000000218494591 ) ) ;
#5149 = CARTESIAN_POINT ( 'NONE',  ( -19.41254052147350961, -21.64274437364857562, 31.61132249208303691 ) ) ;
#5150 = AXIS2_PLACEMENT_3D ( 'NONE', #2756, #7169, #4640 ) ;
#5151 = FACE_OUTER_BOUND ( 'NONE', #2084, .T. ) ;
#5152 = CARTESIAN_POINT ( 'NONE',  ( -9.999999999999994671, -24.16482700510257686, 10.82617750791695777 ) ) ;
#5153 = LINE ( 'NONE', #5063, #9228 ) ;
#5154 = CARTESIAN_POINT ( 'NONE',  ( -9.999999999999994671, -24.16482700510257686, 37.07617750791695954 ) ) ;
#5155 = CARTESIAN_POINT ( 'NONE',  ( -2.500000000000001776, 62.96446609406726225, 46.84999999999998721 ) ) ;
#5156 = CARTESIAN_POINT ( 'NONE',  ( -19.99999999999999645, -24.16482700510261949, 25.92382249208304401 ) ) ;
#5157 = CARTESIAN_POINT ( 'NONE',  ( 2.066987300000001415, 64.00000000000000000, 46.15000000109247225 ) ) ;
#5158 = LINE ( 'NONE', #13876, #12473 ) ;
#5159 = LINE ( 'NONE', #17565, #12575 ) ;
#5160 = CARTESIAN_POINT ( 'NONE',  ( 32.50000000000000000, 47.00000000000000711, -37.50000000000000711 ) ) ;
#5161 = CARTESIAN_POINT ( 'NONE',  ( 2.066987300000001415, 64.00000000000000000, 48.55000000109247082 ) ) ;
#5162 = DIRECTION ( 'NONE',  ( 1.000000000000000000, 0.000000000000000000, 0.000000000000000000 ) ) ;
#5163 = COLOUR_RGB ( '', 0.40784314, 0.44705882, 0.49803922) ;
#5164 = CIRCLE ( 'NONE', #1405, 1.500000000000001332 ) ;
#5165 = VERTEX_POINT ( 'NONE', #11352 ) ;
#5166 = CARTESIAN_POINT ( 'NONE',  ( -18.64274437364860049, -18.02023567606023491, 37.29882249208304046 ) ) ;
#5167 = DIRECTION ( 'NONE',  ( -4.088782444488986608E-17, 0.7071067811865495711, -0.7071067811865455743 ) ) ;
#5168 = CARTESIAN_POINT ( 'NONE',  ( -12.68318583509884157, -21.92450931948787485, 31.16992750791695954 ) ) ;
#5169 = CARTESIAN_POINT ( 'NONE',  ( -41.00000000000000711, 53.00000000000000711, -24.49999999999999645 ) ) ;
#5170 = CARTESIAN_POINT ( 'NONE',  ( -18.35725562635138886, -30.14459132904237393, 19.79882249208303691 ) ) ;
#5171 = CARTESIAN_POINT ( 'NONE',  ( 1.461580736456473684, 65.46158073645646880, 46.05000000109246372 ) ) ;
#5172 = ORIENTED_EDGE ( 'NONE', *, *, #18744, .T. ) ;
#5173 = VERTEX_POINT ( 'NONE', #17345 ) ;
#5174 = PRODUCT_DEFINITION_FORMATION_WITH_SPECIFIED_SOURCE ( 'ANY', '', #12846, .NOT_KNOWN. ) ;
#5175 = DIRECTION ( 'NONE',  ( 1.000000000000000000, -0.000000000000000000, -0.000000000000000000 ) ) ;
#5176 = DIRECTION ( 'NONE',  ( 0.000000000000000000, 0.000000000000000000, 1.000000000000000000 ) ) ;
#5177 = AXIS2_PLACEMENT_3D ( 'NONE', #17459, #8358, #7163 ) ;
#5178 = CARTESIAN_POINT ( 'NONE',  ( 1.461580736456473684, 65.46158073645646880, 46.05000000109246372 ) ) ;
#5179 = CARTESIAN_POINT ( 'NONE',  ( -7.499999999999994671, -38.00000000000000000, 9.500000000000001776 ) ) ;
#5180 = EDGE_CURVE ( 'NONE', #7475, #13902, #2624, .T. ) ;
#5181 = EDGE_CURVE ( 'NONE', #7943, #13315, #14396, .T. ) ;
#5182 = CARTESIAN_POINT ( 'NONE',  ( -0.8561741729129465073, 61.93301270000000613, 45.90000000109247225 ) ) ;
#5183 = LINE ( 'NONE', #17139, #1281 ) ;
#5184 = CARTESIAN_POINT ( 'NONE',  ( 2.500000000000001776, 64.00000000000000000, 47.30000000218494449 ) ) ;
#5185 = ORIENTED_EDGE ( 'NONE', *, *, #2293, .T. ) ;
#5186 = ORIENTED_EDGE ( 'NONE', *, *, #17646, .F. ) ;
#5187 = CARTESIAN_POINT ( 'NONE',  ( -11.35725562635144925, -18.02023567606020293, 36.20117750791695244 ) ) ;
#5188 = VECTOR ( 'NONE', #13405, 1000.000000000000000 ) ;
#5189 = SURFACE_STYLE_USAGE ( .BOTH. , #4092 ) ;
#5190 = EDGE_LOOP ( 'NONE', ( #3893, #1156 ) ) ;
#5191 = VECTOR ( 'NONE', #9273, 1000.000000000000000 ) ;
#5193 = ORIENTED_EDGE ( 'NONE', *, *, #6915, .F. ) ;
#5192 = ORIENTED_EDGE ( 'NONE', *, *, #12749, .T. ) ;
#5194 = CARTESIAN_POINT ( 'NONE',  ( -14.36097942780925685, -20.95583473709189093, 32.70507249208304756 ) ) ;
#5195 = CARTESIAN_POINT ( 'NONE',  ( -21.99999999999999289, -23.83517299489739116, 13.45117750791695777 ) ) ;
#5196 = EDGE_CURVE ( 'NONE', #18345, #11522, #9881, .T. ) ;
#5197 = CARTESIAN_POINT ( 'NONE',  ( 2.492551403682558675, 27.92836399182260720, 58.20336399182267684 ) ) ;
#5198 = CARTESIAN_POINT ( 'NONE',  ( 4.592425496802577917E-16, 61.50000000000000000, 47.90000000218494591 ) ) ;
#5199 = DIRECTION ( 'NONE',  ( -0.000000000000000000, 0.7071067811865456854, 0.7071067811865493491 ) ) ;
#5200 = VERTEX_POINT ( 'NONE', #2261 ) ;
#5201 = EDGE_CURVE ( 'NONE', #2345, #16414, #15876, .T. ) ;
#5202 = CARTESIAN_POINT ( 'NONE',  ( -12.04416526290807887, -24.96867458239596260, 26.79492750791695954 ) ) ;
#5203 = EDGE_CURVE ( 'NONE', #3614, #1662, #14592, .T. ) ;
#5204 = LINE ( 'NONE', #14390, #11593 ) ;
#5205 = ORIENTED_EDGE ( 'NONE', *, *, #9486, .F. ) ;
#5206 = FACE_OUTER_BOUND ( 'NONE', #4400, .T. ) ;
#5207 = VERTEX_POINT ( 'NONE', #17438 ) ;
#5208 = DIRECTION ( 'NONE',  ( -1.000000000000000000, -0.000000000000000000, -0.000000000000000000 ) ) ;
#5209 = CARTESIAN_POINT ( 'NONE',  ( 7.500000000000005329, -38.00000000000000000, 1.500000000000000000 ) ) ;
#5210 = FACE_OUTER_BOUND ( 'NONE', #3101, .T. ) ;
#5211 = AXIS2_PLACEMENT_3D ( 'NONE', #2044, #1955, #10862 ) ;
#5212 = CARTESIAN_POINT ( 'NONE',  ( 3.796994071234847710E-16, 61.93301269999999903, 47.35000000109246798 ) ) ;
#5213 = VECTOR ( 'NONE', #4466, 1000.000000000000000 ) ;
#5214 = CARTESIAN_POINT ( 'NONE',  ( 3.796994071234847710E-16, 61.93301269999999903, 46.75000000109246656 ) ) ;
#5215 = DIRECTION ( 'NONE',  ( 0.000000000000000000, 0.000000000000000000, 1.000000000000000000 ) ) ;
#5216 = DIRECTION ( 'NONE',  ( -1.000000000000000000, 0.000000000000000000, -0.000000000000000000 ) ) ;
#5217 = CARTESIAN_POINT ( 'NONE',  ( -1.040834085586084257E-14, 25.49999999999998934, 52.50000000000000711 ) ) ;
#5218 = EDGE_LOOP ( 'NONE', ( #130, #3334, #1580, #15814 ) ) ;
#5219 = ORIENTED_EDGE ( 'NONE', *, *, #7105, .F. ) ;
#5220 = CARTESIAN_POINT ( 'NONE',  ( -9.999999999999994671, -24.16482700510257686, 26.57617750791695954 ) ) ;
#5221 = DIRECTION ( 'NONE',  ( 0.000000000000000000, -1.000000000000000000, 0.000000000000000000 ) ) ;
#5222 = EDGE_LOOP ( 'NONE', ( #18536, #8538 ) ) ;
#5223 = CARTESIAN_POINT ( 'NONE',  ( -10.58745947852648328, -26.35725562635138530, 28.98632249208304401 ) ) ;
#5224 = VECTOR ( 'NONE', #15223, 1000.000000000000000 ) ;
#5225 = EDGE_CURVE ( 'NONE', #10014, #3695, #1065, .T. ) ;
#5226 = AXIS2_PLACEMENT_3D ( 'NONE', #18593, #3683, #2019 ) ;
#5227 = CARTESIAN_POINT ( 'NONE',  ( 2.500000000000001776, 65.03553390593273775, 45.64999999999999147 ) ) ;
#5228 = CARTESIAN_POINT ( 'NONE',  ( -11.99999999999999289, -23.83517299489735564, 28.54882249208304046 ) ) ;
#5229 = CARTESIAN_POINT ( 'NONE',  ( -0.1250000000000104083, 33.66708332270461312, 52.46464466094069934 ) ) ;
#5230 = VERTEX_POINT ( 'NONE', #16063 ) ;
#5231 = CARTESIAN_POINT ( 'NONE',  ( 34.99999999999999289, -6.000000000000000000, 42.49999999999997868 ) ) ;
#5232 = ORIENTED_EDGE ( 'NONE', *, *, #17550, .F. ) ;
#5233 = CARTESIAN_POINT ( 'NONE',  ( 49.99999999999998579, 3.000000000000000000, 59.99999999999997868 ) ) ;
#5234 = EDGE_CURVE ( 'NONE', #18711, #14054, #8609, .T. ) ;
#5235 = DIRECTION ( 'NONE',  ( 0.000000000000000000, 0.000000000000000000, -1.000000000000000000 ) ) ;
#5236 = CARTESIAN_POINT ( 'NONE',  ( 44.99999999999997158, 3.000000000000000000, 56.50000000000000000 ) ) ;
#5237 = AXIS2_PLACEMENT_3D ( 'NONE', #7255, #14995, #7545 ) ;
#5238 = VECTOR ( 'NONE', #9926, 1000.000000000000000 ) ;
#5239 = CARTESIAN_POINT ( 'NONE',  ( -7.999999999999996447, -25.00000000000000711, 1.500000000000000000 ) ) ;
#5240 = DIRECTION ( 'NONE',  ( 0.000000000000000000, 1.000000000000000000, 0.000000000000000000 ) ) ;
#5241 = PLANE ( 'NONE',  #11753 ) ;
#5242 = ADVANCED_FACE ( 'NONE', ( #11640 ), #17631, .T. ) ;
#5243 = EDGE_LOOP ( 'NONE', ( #4302, #11093, #10680, #16355 ) ) ;
#5244 = CARTESIAN_POINT ( 'NONE',  ( -19.99999999999999645, -23.83517299489738051, 34.45117750791696665 ) ) ;
#5245 = CARTESIAN_POINT ( 'NONE',  ( 1.461580736456473906, 62.53841926354353120, 47.45000000109246940 ) ) ;
#5246 = CARTESIAN_POINT ( 'NONE',  ( -19.24771351637086880, -26.64274437364857206, 30.73632249208304401 ) ) ;
#5247 = STYLED_ITEM ( 'NONE', ( #14778 ), #12018 ) ;
#5248 = CARTESIAN_POINT ( 'NONE',  ( -41.00000000000000711, 110.0000000000000000, 14.50000000000000000 ) ) ;
#5249 = CARTESIAN_POINT ( 'NONE',  ( -12.64274437364855252, -28.41254052147347053, 27.45117750791695954 ) ) ;
#5250 = DIRECTION ( 'NONE',  ( -0.000000000000000000, -0.000000000000000000, -1.000000000000000000 ) ) ;
#5251 = CARTESIAN_POINT ( 'NONE',  ( -18.78091578003889595, -27.53959229564985023, 28.54492750791695954 ) ) ;
#5252 = LINE ( 'NONE', #2391, #10272 ) ;
#5253 = CARTESIAN_POINT ( 'NONE',  ( -13.49542703274174116, -28.95583473709188738, 29.64257249208304046 ) ) ;
#5254 = CARTESIAN_POINT ( 'NONE',  ( 2.500000000000001776, 64.00000000000000000, 48.79999999999999716 ) ) ;
#5255 = CARTESIAN_POINT ( 'NONE',  ( -2.066987300000001415, 64.00000000000000000, 48.95000000109246940 ) ) ;
#5256 = FILL_AREA_STYLE_COLOUR ( '', #6784 ) ;
#5257 = CARTESIAN_POINT ( 'NONE',  ( 3.796994071234847710E-16, 61.93301269999999903, 45.95000000109246940 ) ) ;
#5258 = LINE ( 'NONE', #12692, #12700 ) ;
#5259 = ORIENTED_EDGE ( 'NONE', *, *, #17753, .T. ) ;
#5260 = CARTESIAN_POINT ( 'NONE',  ( 3.796994071234847710E-16, 61.93301269999999903, 46.55000000109247082 ) ) ;
#5261 = CARTESIAN_POINT ( 'NONE',  ( -13.64274437364856141, -26.68048971390460622, 32.70117750791696665 ) ) ;
#5262 = CARTESIAN_POINT ( 'NONE',  ( -45.00000000000000000, 3.000000000000000000, 53.49999999999998579 ) ) ;
#5263 = CARTESIAN_POINT ( 'NONE',  ( -11.35725562635139418, -29.97976432393972601, 34.67382249208304046 ) ) ;
#5264 = CARTESIAN_POINT ( 'NONE',  ( -1.461580736456473906, 65.46158073645646880, 47.85000000109246798 ) ) ;
#5265 = ORIENTED_EDGE ( 'NONE', *, *, #11090, .F. ) ;
#5266 =( BOUNDED_CURVE ( )  B_SPLINE_CURVE ( 2, ( #740, #14074, #4971, #15551, #1828, #6346, #3302, #10835, #9271 ),
 .UNSPECIFIED., .F., .F. ) 
 B_SPLINE_CURVE_WITH_KNOTS ( ( 3, 2, 2, 2, 3 ),
 ( 0.1428571428571428215, 0.1607142857142856429, 0.1785714285714284644, 0.1964285714285712858, 0.2142857142857140795 ),
 .UNSPECIFIED. ) 
 CURVE ( )  GEOMETRIC_REPRESENTATION_ITEM ( )  RATIONAL_B_SPLINE_CURVE ( ( 1.000000000000000222, 0.9238795325112866275, 1.000000000000000000, 0.9238795325112867385, 1.000000000000000000, 0.9238795325112867385, 1.000000000000000000, 0.9238795325112875156, 0.9999999999999992228 ) ) 
 REPRESENTATION_ITEM ( '' )  );
#5267 = DIRECTION ( 'NONE',  ( -4.898042755699219393E-16, 0.000000000000000000, -1.000000000000000000 ) ) ;
#5268 = CARTESIAN_POINT ( 'NONE',  ( -1.040834085586084257E-14, 29.74264068711926257, 56.74264068711929809 ) ) ;
#5269 = CARTESIAN_POINT ( 'NONE',  ( 1.461580736456473906, 62.53841926354353120, 45.05000000109246372 ) ) ;
#5270 = CARTESIAN_POINT ( 'NONE',  ( -14.99999999999999645, 73.00000000000001421, 23.99999999999997868 ) ) ;
#5271 = CARTESIAN_POINT ( 'NONE',  ( 2.500000000000000000, -1.178949249685214307, 2.042000000000002036 ) ) ;
#5272 = LINE ( 'NONE', #9770, #4573 ) ;
#5273 = VERTEX_POINT ( 'NONE', #12735 ) ;
#5274 = ORIENTED_EDGE ( 'NONE', *, *, #16091, .T. ) ;
#5275 = CARTESIAN_POINT ( 'NONE',  ( -9.020235676060220698, -27.64274437364852588, 27.01367750791695599 ) ) ;
#5276 = ORIENTED_EDGE ( 'NONE', *, *, #5604, .T. ) ;
#5278 = EDGE_LOOP ( 'NONE', ( #1697, #8501, #9253, #15208 ) ) ;
#5277 = ORIENTED_EDGE ( 'NONE', *, *, #9391, .F. ) ;
#5279 = CARTESIAN_POINT ( 'NONE',  ( -17.95583473709190869, -24.96867458239598037, 25.70507249208304756 ) ) ;
#5280 = ADVANCED_FACE ( 'NONE', ( #18731 ), #13211, .T. ) ;
#5281 = EDGE_CURVE ( 'NONE', #10345, #13549, #9972, .T. ) ;
#5282 = CARTESIAN_POINT ( 'NONE',  ( -20.00369391078762860, -18.75498260482333279, 29.85742750791695599 ) ) ;
#5283 = CARTESIAN_POINT ( 'NONE',  ( -8.528048594804062077, -42.28611686177728046, 1.500000000000000000 ) ) ;
#5284 = CARTESIAN_POINT ( 'NONE',  ( 1.767766952966369987, 65.76776695296638309, 47.40000000218494591 ) ) ;
#5285 = DIRECTION ( 'NONE',  ( -8.177564888977974449E-17, -0.7071067811865495711, 0.7071067811865455743 ) ) ;
#5286 = ORIENTED_EDGE ( 'NONE', *, *, #1820, .T. ) ;
#5287 = CARTESIAN_POINT ( 'NONE',  ( -14.83517299489738761, -20.99999999999997513, 30.51367750791696309 ) ) ;
#5288 = EDGE_CURVE ( 'NONE', #13466, #13503, #7334, .T. ) ;
#5289 = FACE_OUTER_BOUND ( 'NONE', #8515, .T. ) ;
#5290 = EDGE_LOOP ( 'NONE', ( #8510, #18971 ) ) ;
#5291 = LINE ( 'NONE', #9878, #11557 ) ;
#5292 = ORIENTED_EDGE ( 'NONE', *, *, #7515, .F. ) ;
#5293 = LINE ( 'NONE', #4110, #4760 ) ;
#5294 = CARTESIAN_POINT ( 'NONE',  ( -35.00000000000002132, -6.000000000000000000, -42.50000000000001421 ) ) ;
#5295 = FACE_BOUND ( 'NONE', #13993, .T. ) ;
#5296 = EDGE_CURVE ( 'NONE', #11714, #12973, #8806, .T. ) ;
#5297 = CIRCLE ( 'NONE', #4684, 2.499999999999998668 ) ;
#5298 = CARTESIAN_POINT ( 'NONE',  ( 0.8561741729129472844, 61.93301270000000613, 45.80000000109246372 ) ) ;
#5299 = CARTESIAN_POINT ( 'NONE',  ( 0.8561741729129471734, 61.93301270000000613, 49.20000000109247651 ) ) ;
#5300 = DIRECTION ( 'NONE',  ( 0.000000000000000000, 0.000000000000000000, -1.000000000000000000 ) ) ;
#5301 = VECTOR ( 'NONE', #12684, 1000.000000000000000 ) ;
#5302 = CYLINDRICAL_SURFACE ( 'NONE', #11775, 2.500000000000001776 ) ;
#5303 = LINE ( 'NONE', #2169, #6123 ) ;
#5304 = ORIENTED_EDGE ( 'NONE', *, *, #12384, .F. ) ;
#5305 = ORIENTED_EDGE ( 'NONE', *, *, #13190, .F. ) ;
#5306 = CARTESIAN_POINT ( 'NONE',  ( -18.53959229564986799, -20.21908421996107563, 29.85742750791695599 ) ) ;
#5307 = DIRECTION ( 'NONE',  ( 0.000000000000000000, 0.000000000000000000, -1.000000000000000000 ) ) ;
#5308 = ORIENTED_EDGE ( 'NONE', *, *, #8762, .T. ) ;
#5309 = CARTESIAN_POINT ( 'NONE',  ( -11.21908421996106320, -27.53959229564982181, 34.45507249208304046 ) ) ;
#5310 = VECTOR ( 'NONE', #5167, 1000.000000000000114 ) ;
#5311 = CARTESIAN_POINT ( 'NONE',  ( 1.300000000000000044, -0.7390083445627200209, 1.280000000000001137 ) ) ;
#5312 = CARTESIAN_POINT ( 'NONE',  ( -17.68048971390462754, -22.64274437364856496, 26.36132249208304401 ) ) ;
#5313 = AXIS2_PLACEMENT_3D ( 'NONE', #6411, #1799, #3368 ) ;
#5314 = PRESENTATION_STYLE_ASSIGNMENT (( #7062 ) ) ;
#5315 = VERTEX_POINT ( 'NONE', #13302 ) ;
#5316 = VECTOR ( 'NONE', #13700, 1000.000000000000000 ) ;
#5317 = CARTESIAN_POINT ( 'NONE',  ( -47.00000000000001421, 30.00000000000000355, 37.49999999999996447 ) ) ;
#5318 = ORIENTED_EDGE ( 'NONE', *, *, #12280, .F. ) ;
#5319 = DIRECTION ( 'NONE',  ( 1.000000000000000000, 0.000000000000000000, -5.782411586589357392E-17 ) ) ;
#5320 = CARTESIAN_POINT ( 'NONE',  ( -4.012830983233618198, 32.52836399182267257, 53.60336399182263989 ) ) ;
#5321 = DIRECTION ( 'NONE',  ( -0.000000000000000000, -1.000000000000000000, -0.000000000000000000 ) ) ;
#5322 = AXIS2_PLACEMENT_3D ( 'NONE', #6283, #5111, #7951 ) ;
#5323 = VECTOR ( 'NONE', #9994, 1000.000000000000000 ) ;
#5324 = EDGE_CURVE ( 'NONE', #13252, #14588, #17728, .T. ) ;
#5325 = EDGE_CURVE ( 'NONE', #4512, #10175, #5871, .T. ) ;
#5326 = SURFACE_SIDE_STYLE ('',( #14331 ) ) ;
#5327 = CARTESIAN_POINT ( 'NONE',  ( -4.012830983233701687, 26.60336399182265055, 59.52836399182262994 ) ) ;
#5328 = EDGE_CURVE ( 'NONE', #5928, #6595, #18465, .T. ) ;
#5329 = LINE ( 'NONE', #11193, #15843 ) ;
#5330 = VECTOR ( 'NONE', #4922, 1000.000000000000000 ) ;
#5331 = DIRECTION ( 'NONE',  ( -1.000000000000000000, 0.000000000000000000, -0.000000000000000000 ) ) ;
#5332 = EDGE_LOOP ( 'NONE', ( #376, #6836, #13310, #18830 ) ) ;
#5333 = EDGE_CURVE ( 'NONE', #1158, #14224, #18089, .T. ) ;
#5334 = CARTESIAN_POINT ( 'NONE',  ( -12.35725562635143682, -19.75228648362908501, 25.70117750791695599 ) ) ;
#5335 = CIRCLE ( 'NONE', #1590, 1.500000000000001332 ) ;
#5336 = CARTESIAN_POINT ( 'NONE',  ( 2.066987300000002303, 63.14382582708705627, 46.70000000109248361 ) ) ;
#5337 = CARTESIAN_POINT ( 'NONE',  ( -10.58745947852648328, -26.35725562635138530, 39.48632249208304046 ) ) ;
#5338 = DIRECTION ( 'NONE',  ( 0.000000000000000000, -1.000000000000000000, 0.000000000000000000 ) ) ;
#5339 = CARTESIAN_POINT ( 'NONE',  ( -17.35725562635144215, -19.58745947852648683, 30.07617750791695599 ) ) ;
#5340 = LINE ( 'NONE', #11587, #4537 ) ;
#5341 = CARTESIAN_POINT ( 'NONE',  ( -18.78091578003889595, -27.53959229564985023, 39.04492750791695954 ) ) ;
#5342 = VECTOR ( 'NONE', #6591, 1000.000000000000000 ) ;
#5343 = CARTESIAN_POINT ( 'NONE',  ( -41.00000000000000711, 53.00000000000000711, 0.5000000000000004441 ) ) ;
#5344 = CARTESIAN_POINT ( 'NONE',  ( -19.24771351637086880, -26.64274437364857206, 20.23632249208304046 ) ) ;
#5345 = EDGE_CURVE ( 'NONE', #1624, #964, #14984, .T. ) ;
#5346 = ADVANCED_FACE ( 'NONE', ( #16361 ), #13743, .F. ) ;
#5347 = CARTESIAN_POINT ( 'NONE',  ( 2.066987300000002303, 63.14382582708705627, 46.10000000109246798 ) ) ;
#5348 = CARTESIAN_POINT ( 'NONE',  ( 0.000000000000000000, 64.00000000000000000, 49.99999999999999289 ) ) ;
#5349 = VECTOR ( 'NONE', #12818, 1000.000000000000114 ) ;
#5350 = CARTESIAN_POINT ( 'NONE',  ( -44.99999999999998579, 3.000000000000000000, -56.50000000000000000 ) ) ;
#5351 = CARTESIAN_POINT ( 'NONE',  ( 0.8561741729129472844, 61.93301270000000613, 45.20000000109248361 ) ) ;
#5352 = DIRECTION ( 'NONE',  ( 0.000000000000000000, -1.000000000000000000, 0.000000000000000000 ) ) ;
#5353 = VECTOR ( 'NONE', #14819, 1000.000000000000000 ) ;
#5354 = B_SPLINE_CURVE_WITH_KNOTS ( 'NONE', 1,
 ( #8727, #1293 ),
 .UNSPECIFIED., .F., .F.,
 ( 2, 2 ),
 ( 0.000000000000000000, 1.000000000000000000 ),
 .UNSPECIFIED. ) ;
#5355 = ORIENTED_EDGE ( 'NONE', *, *, #4279, .T. ) ;
#5356 = VECTOR ( 'NONE', #18528, 1000.000000000000000 ) ;
#5357 =( NAMED_UNIT ( * ) PLANE_ANGLE_UNIT ( ) SI_UNIT ( $, .RADIAN. ) );
#5358 = CARTESIAN_POINT ( 'NONE',  ( -2.066987300000001415, 64.00000000000000000, 44.75000000109247367 ) ) ;
#5359 = CARTESIAN_POINT ( 'NONE',  ( -11.21908421996108629, -20.46040770435011069, 4.919927507916955989 ) ) ;
#5360 = DIRECTION ( 'NONE',  ( 0.000000000000000000, -1.000000000000000000, -0.000000000000000000 ) ) ;
#5361 = CARTESIAN_POINT ( 'NONE',  ( -15.16482700510264436, -16.99999999999997868, 27.23632249208303691 ) ) ;
#5362 = AXIS2_PLACEMENT_3D ( 'NONE', #8243, #17158, #2430 ) ;
#5363 = CARTESIAN_POINT ( 'NONE',  ( -2.066987300000001859, 64.85617417291294373, 48.90000000109247225 ) ) ;
#5364 = EDGE_LOOP ( 'NONE', ( #10754, #13809, #2711, #9469, #12213, #7654, #3655, #2400, #2819, #2556, #1072, #15373, #4150, #9302, #16672 ) ) ;
#5365 = CARTESIAN_POINT ( 'NONE',  ( -10.00000000000000000, -35.74454190283286437, 7.499999999999996447 ) ) ;
#5366 = DIRECTION ( 'NONE',  ( 0.000000000000000000, 1.000000000000000000, 0.000000000000000000 ) ) ;
#5367 = VECTOR ( 'NONE', #9813, 1000.000000000000000 ) ;
#5368 = EDGE_CURVE ( 'NONE', #14967, #9993, #11942, .T. ) ;
#5369 = CARTESIAN_POINT ( 'NONE',  ( 2.066987300000001859, 63.14382582708704916, 45.10000000109246798 ) ) ;
#5370 = LINE ( 'NONE', #18794, #7462 ) ;
#5371 = VECTOR ( 'NONE', #8182, 1000.000000000000000 ) ;
#5372 = CARTESIAN_POINT ( 'NONE',  ( 4.592425496802577917E-16, 61.50000000000000000, 47.79999999999999716 ) ) ;
#5373 = CARTESIAN_POINT ( 'NONE',  ( 21.49999999999997513, 118.0000000000000142, -52.50000000000002132 ) ) ;
#5374 = AXIS2_PLACEMENT_3D ( 'NONE', #16130, #17228, #17604 ) ;
#5375 = DIRECTION ( 'NONE',  ( -0.000000000000000000, 0.7071067811865452413, 0.7071067811865497932 ) ) ;
#5376 = EDGE_LOOP ( 'NONE', ( #3078, #10156, #5705, #14633 ) ) ;
#5377 = EDGE_LOOP ( 'NONE', ( #5906, #19115, #6837, #14115, #5185, #14018 ) ) ;
#5378 = CARTESIAN_POINT ( 'NONE',  ( -14.83517299489740715, -16.99999999999997868, 41.01367750791695954 ) ) ;
#5379 = VECTOR ( 'NONE', #2995, 1000.000000000000000 ) ;
#5380 = ORIENTED_EDGE ( 'NONE', *, *, #4533, .F. ) ;
#5382 = ORIENTED_EDGE ( 'NONE', *, *, #14905, .F. ) ;
#5381 = ORIENTED_EDGE ( 'NONE', *, *, #11287, .T. ) ;
#5383 = CARTESIAN_POINT ( 'NONE',  ( -12.31951028609537602, -22.64274437364854364, 5.138677507916959541 ) ) ;
#5384 = CARTESIAN_POINT ( 'NONE',  ( -16.71081734191527346, -16.95583473709190159, 25.04492750791695599 ) ) ;
#5385 = VECTOR ( 'NONE', #15271, 1000.000000000000000 ) ;
#5386 = PLANE ( 'NONE',  #17911 ) ;
#5387 = CARTESIAN_POINT ( 'NONE',  ( -1.530808498934192803E-16, 66.50000000000000000, 48.30000000218494449 ) ) ;
#5388 = FACE_OUTER_BOUND ( 'NONE', #11150, .T. ) ;
#5389 = ORIENTED_EDGE ( 'NONE', *, *, #10675, .T. ) ;
#5390 = CARTESIAN_POINT ( 'NONE',  ( -9.673552776372430100E-15, -37.75835931288066405, -19.24364068711958708 ) ) ;
#5391 = ORIENTED_EDGE ( 'NONE', *, *, #12620, .F. ) ;
#5392 = EDGE_CURVE ( 'NONE', #7133, #15771, #6171, .T. ) ;
#5393 = CARTESIAN_POINT ( 'NONE',  ( -4.189607678530337331, 26.72836399182265055, 59.40336399182262284 ) ) ;
#5394 = ORIENTED_EDGE ( 'NONE', *, *, #11769, .F. ) ;
#5395 = PLANE ( 'NONE',  #8802 ) ;
#5396 = PLANE ( 'NONE',  #12789 ) ;
#5397 = DIRECTION ( 'NONE',  ( -1.156482317317871478E-16, 1.000000000000000000, 0.000000000000000000 ) ) ;
#5398 = CARTESIAN_POINT ( 'NONE',  ( 2.066987300000001415, 64.00000000000000000, 45.15000000109247225 ) ) ;
#5399 = DIRECTION ( 'NONE',  ( -0.000000000000000000, -1.000000000000000000, -0.000000000000000000 ) ) ;
#5400 = VECTOR ( 'NONE', #16653, 1000.000000000000000 ) ;
#5401 = CARTESIAN_POINT ( 'NONE',  ( -2.500000000000001776, 64.00000000000000000, 46.90000000218494591 ) ) ;
#5402 = CARTESIAN_POINT ( 'NONE',  ( 2.336416577439934805, 64.02633867252365008, 44.99999999999999289 ) ) ;
#5403 = VERTEX_POINT ( 'NONE', #1558 ) ;
#5404 = EDGE_LOOP ( 'NONE', ( #3525, #11161 ) ) ;
#5405 = CARTESIAN_POINT ( 'NONE',  ( -21.99999999999999289, -23.83517299489739116, 2.951177507916956433 ) ) ;
#5406 = LINE ( 'NONE', #985, #9277 ) ;
#5407 = ORIENTED_EDGE ( 'NONE', *, *, #9343, .T. ) ;
#5408 = CARTESIAN_POINT ( 'NONE',  ( -13.49542703274174116, -28.95583473709188738, 34.89257249208304046 ) ) ;
#5409 = CARTESIAN_POINT ( 'NONE',  ( -2.500000000000000888, 62.96446609406726935, 45.24999999999999289 ) ) ;
#5410 = ORIENTED_EDGE ( 'NONE', *, *, #5920, .F. ) ;
#5411 = EDGE_CURVE ( 'NONE', #9204, #9159, #16575, .T. ) ;
#5412 = CARTESIAN_POINT ( 'NONE',  ( -12.68318583509882380, -26.07549068051207541, 29.20507249208304756 ) ) ;
#5413 = DIRECTION ( 'NONE',  ( 1.000000000000000000, 0.000000000000000000, 0.000000000000000000 ) ) ;
#5414 = ORIENTED_EDGE ( 'NONE', *, *, #1203, .F. ) ;
#5415 = DIRECTION ( 'NONE',  ( 0.000000000000000000, 0.000000000000000000, 1.000000000000000000 ) ) ;
#5416 = ORIENTED_EDGE ( 'NONE', *, *, #5451, .T. ) ;
#5417 = CARTESIAN_POINT ( 'NONE',  ( -1.035533905932738641, 66.50000000000000000, 45.15000000218493881 ) ) ;
#5418 = LINE ( 'NONE', #11374, #160 ) ;
#5419 = CARTESIAN_POINT ( 'NONE',  ( 41.00000000000000000, 52.00000000000000711, 18.00000000000000000 ) ) ;
#5420 = ADVANCED_FACE ( 'NONE', ( #10159 ), #16159, .T. ) ;
#5421 = CARTESIAN_POINT ( 'NONE',  ( -20.04416526290808065, -25.17491895705300209, 23.73242750791694888 ) ) ;
#5422 = PRESENTATION_STYLE_ASSIGNMENT (( #901 ) ) ;
#5423 = SURFACE_STYLE_USAGE ( .BOTH. , #811 ) ;
#5424 = DIRECTION ( 'NONE',  ( -1.000000000000000000, 0.000000000000000000, -0.000000000000000000 ) ) ;
#5425 = LINE ( 'NONE', #11382, #12086 ) ;
#5426 = ORIENTED_EDGE ( 'NONE', *, *, #14108, .T. ) ;
#5427 = CARTESIAN_POINT ( 'NONE',  ( -18.78091578003889950, -27.53959229564985378, 28.54492750791695954 ) ) ;
#5428 = CARTESIAN_POINT ( 'NONE',  ( -2.066987300000001415, 64.00000000000000000, 48.75000000109246656 ) ) ;
#5429 = CARTESIAN_POINT ( 'NONE',  ( -14.83517299489735741, -28.99999999999998224, 35.11132249208304046 ) ) ;
#5430 = CARTESIAN_POINT ( 'NONE',  ( 2.500000000000007994, 62.96446609406726225, 48.74999999999999289 ) ) ;
#5431 = EDGE_CURVE ( 'NONE', #15167, #15535, #1543, .T. ) ;
#5432 = ADVANCED_FACE ( 'NONE', ( #1754 ), #9484, .T. ) ;
#5433 = PLANE ( 'NONE',  #6588 ) ;
#5434 = CARTESIAN_POINT ( 'NONE',  ( -18.53959229564986799, -20.21908421996107563, 35.10742750791694533 ) ) ;
#5435 = ADVANCED_FACE ( 'NONE', ( #3517 ), #6367, .T. ) ;
#5436 = DIRECTION ( 'NONE',  ( -1.000000000000000000, 0.000000000000000000, -0.000000000000000000 ) ) ;
#5437 = CARTESIAN_POINT ( 'NONE',  ( -11.46040770435012490, -27.78091578003888173, 32.48242750791695954 ) ) ;
#5438 = LINE ( 'NONE', #12874, #13411 ) ;
#5439 = DIRECTION ( 'NONE',  ( -0.7071067811865487940, -0.5000000000000003331, 0.4999999999999979461 ) ) ;
#5440 =( REPRESENTATION_RELATIONSHIP ('NONE','NONE', #7912, #6533 ) REPRESENTATION_RELATIONSHIP_WITH_TRANSFORMATION ( #312 )SHAPE_REPRESENTATION_RELATIONSHIP( ) );
#5441 = CARTESIAN_POINT ( 'NONE',  ( -1.461580736456473462, 62.53841926354353120, 45.85000000109246798 ) ) ;
#5442 = CARTESIAN_POINT ( 'NONE',  ( -1.461580736456473906, 65.46158073645646880, 48.85000000109246798 ) ) ;
#5443 = CARTESIAN_POINT ( 'NONE',  ( 44.99999999999997158, 0.000000000000000000, 55.00000000000000000 ) ) ;
#5444 = CARTESIAN_POINT ( 'NONE',  ( -2.500000000000001776, 64.00000000000000000, 49.99999999999999289 ) ) ;
#5445 = CARTESIAN_POINT ( 'NONE',  ( -50.00000000000001421, 3.000000000000000000, 59.99999999999997868 ) ) ;
#5446 = ORIENTED_EDGE ( 'NONE', *, *, #2495, .F. ) ;
#5447 = CARTESIAN_POINT ( 'NONE',  ( -1.265664690411616068E-16, 66.06698730000000808, 45.35000000109246798 ) ) ;
#5448 = CARTESIAN_POINT ( 'NONE',  ( -12.31951028609537602, -22.64274437364854364, 36.63867750791695244 ) ) ;
#5449 = CARTESIAN_POINT ( 'NONE',  ( 44.99999999999997158, 0.000000000000000000, 55.00000000000000000 ) ) ;
#5450 = CARTESIAN_POINT ( 'NONE',  ( -14.83517299489734853, -30.99999999999998224, 35.11132249208304046 ) ) ;
#5451 = EDGE_CURVE ( 'NONE', #19196, #14374, #8122, .T. ) ;
#5452 = CARTESIAN_POINT ( 'NONE',  ( 2.066987300000001859, 64.85617417291294373, 47.80000000109247082 ) ) ;
#5453 = ORIENTED_EDGE ( 'NONE', *, *, #1812, .T. ) ;
#5454 = CARTESIAN_POINT ( 'NONE',  ( 47.00000000000000000, 115.0000000000000000, -56.99999999999999289 ) ) ;
#5455 = DIRECTION ( 'NONE',  ( -0.000000000000000000, 1.000000000000000000, -0.000000000000000000 ) ) ;
#5456 = CARTESIAN_POINT ( 'NONE',  ( -0.8561741729129461742, 66.06698730000000808, 46.20000000109248361 ) ) ;
#5457 = DIRECTION ( 'NONE',  ( 0.000000000000000000, 0.000000000000000000, 1.000000000000000000 ) ) ;
#5458 = DIRECTION ( 'NONE',  ( 0.000000000000000000, -0.5000000000000013323, -0.8660254037844378194 ) ) ;
#5459 = PLANE ( 'NONE',  #5655 ) ;
#5460 = DIRECTION ( 'NONE',  ( -0.000000000000000000, 0.000000000000000000, 1.000000000000000000 ) ) ;
#5461 = ORIENTED_EDGE ( 'NONE', *, *, #12471, .F. ) ;
#5462 = VERTEX_POINT ( 'NONE', #15568 ) ;
#5463 = CARTESIAN_POINT ( 'NONE',  ( -9.996306089212408708, -18.75498260482328661, 1.642572492083039126 ) ) ;
#5464 = ORIENTED_EDGE ( 'NONE', *, *, #7592, .F. ) ;
#5466 = ORIENTED_EDGE ( 'NONE', *, *, #4960, .F. ) ;
#5465 = ORIENTED_EDGE ( 'NONE', *, *, #11049, .F. ) ;
#5467 = EDGE_CURVE ( 'NONE', #19215, #7148, #15379, .T. ) ;
#5468 = CARTESIAN_POINT ( 'NONE',  ( -15.96867458239597326, -26.95583473709190159, 1.857427507916959986 ) ) ;
#5469 = CARTESIAN_POINT ( 'NONE',  ( -21.14459132904236327, -27.35725562635143149, 34.01367750791695244 ) ) ;
#5470 = AXIS2_PLACEMENT_3D ( 'NONE', #7695, #13763, #16618 ) ;
#5471 = AXIS2_PLACEMENT_3D ( 'NONE', #3863, #2673, #15822 ) ;
#5472 = LINE ( 'NONE', #7033, #14456 ) ;
#5473 = CARTESIAN_POINT ( 'NONE',  ( -1.767766952966370209, 65.76776695296638309, 46.80000000218494449 ) ) ;
#5474 = LINE ( 'NONE', #15962, #16603 ) ;
#5475 = ORIENTED_EDGE ( 'NONE', *, *, #7103, .T. ) ;
#5476 = CARTESIAN_POINT ( 'NONE',  ( -4.101219330881938241, 32.64264068711930378, 53.84264068711927109 ) ) ;
#5477 = VERTEX_POINT ( 'NONE', #13896 ) ;
#5478 = CARTESIAN_POINT ( 'NONE',  ( -1.040834085586084257E-14, 30.30832611206852079, 47.69167388793148632 ) ) ;
#5479 = VERTEX_POINT ( 'NONE', #14094 ) ;
#5480 = CARTESIAN_POINT ( 'NONE',  ( 0.000000000000000000, 64.00000000000000000, 49.99999999999999289 ) ) ;
#5481 = ADVANCED_FACE ( 'NONE', ( #2137 ), #11047, .F. ) ;
#5482 = DIRECTION ( 'NONE',  ( 0.000000000000000000, 0.000000000000000000, -1.000000000000000000 ) ) ;
#5483 = DIRECTION ( 'NONE',  ( -1.000000000000000000, -0.000000000000000000, -0.000000000000000000 ) ) ;
#5484 = CARTESIAN_POINT ( 'NONE',  ( -1.265664690411616068E-16, 66.06698730000000808, 46.15000000109247225 ) ) ;
#5485 = CARTESIAN_POINT ( 'NONE',  ( 0.000000000000000000, -52.00000000000000711, 1.500000000000000000 ) ) ;
#5486 = AXIS2_PLACEMENT_3D ( 'NONE', #5637, #4468, #16322 ) ;
#5487 = CARTESIAN_POINT ( 'NONE',  ( -2.500000000000001776, 64.00000000000000000, 46.10000000218494165 ) ) ;
#5488 = VECTOR ( 'NONE', #2374, 1000.000000000000000 ) ;
#5489 = CARTESIAN_POINT ( 'NONE',  ( 0.1249999999999895917, 33.66708332270461312, 52.46464466094069934 ) ) ;
#5490 = ORIENTED_EDGE ( 'NONE', *, *, #4037, .T. ) ;
#5491 = ORIENTED_EDGE ( 'NONE', *, *, #7649, .T. ) ;
#5492 = CARTESIAN_POINT ( 'NONE',  ( -20.00369391078762860, -18.75498260482333279, 8.857427507916955989 ) ) ;
#5493 = CARTESIAN_POINT ( 'NONE',  ( -40.00000000000000000, 53.00000000000000711, 6.999999999999999112 ) ) ;
#5494 = ORIENTED_EDGE ( 'NONE', *, *, #8435, .T. ) ;
#5495 = CARTESIAN_POINT ( 'NONE',  ( -12.31951028609536536, -25.35725562635139596, 2.736322492083043123 ) ) ;
#5496 = CARTESIAN_POINT ( 'NONE',  ( -2.500000000000001776, 65.03553390593273775, 45.95000000000000995 ) ) ;
#5497 = ORIENTED_EDGE ( 'NONE', *, *, #17416, .F. ) ;
#5498 = CARTESIAN_POINT ( 'NONE',  ( -14.83517299489736985, -26.99999999999998579, 35.11132249208304756 ) ) ;
#5499 = VECTOR ( 'NONE', #4538, 1000.000000000000000 ) ;
#5500 =( NAMED_UNIT ( * ) PLANE_ANGLE_UNIT ( ) SI_UNIT ( $, .RADIAN. ) );
#5501 = VERTEX_POINT ( 'NONE', #7835 ) ;
#5502 = PLANE ( 'NONE',  #11873 ) ;
#5503 = ORIENTED_EDGE ( 'NONE', *, *, #12877, .F. ) ;
#5504 = PLANE ( 'NONE',  #14703 ) ;
#5505 = LINE ( 'NONE', #6793, #13292 ) ;
#5506 = LINE ( 'NONE', #1184, #17878 ) ;
#5507 = PLANE ( 'NONE',  #4446 ) ;
#5508 = CARTESIAN_POINT ( 'NONE',  ( -10.04416526290807710, -25.50457296725819489, 26.79492750791695954 ) ) ;
#5509 = DIRECTION ( 'NONE',  ( 0.000000000000000000, 1.000000000000000000, 0.000000000000000000 ) ) ;
#5510 = DIRECTION ( 'NONE',  ( 0.000000000000000000, 0.000000000000000000, -1.000000000000000000 ) ) ;
#5511 = CARTESIAN_POINT ( 'NONE',  ( -10.58745947852649927, -21.64274437364853654, -0.1113224920830418047 ) ) ;
#5512 = VECTOR ( 'NONE', #4386, 1000.000000000000000 ) ;
#5513 = CARTESIAN_POINT ( 'NONE',  ( 2.500000000000001776, 64.00000000000000000, 45.59999999999999432 ) ) ;
#5514 = ORIENTED_EDGE ( 'NONE', *, *, #19178, .T. ) ;
#5515 = VECTOR ( 'NONE', #833, 1000.000000000000000 ) ;
#5516 = UNCERTAINTY_MEASURE_WITH_UNIT (LENGTH_MEASURE( 1.000000000000000082E-05 ), #2713, 'distance_accuracy_value', 'NONE');
#5517 = CARTESIAN_POINT ( 'NONE',  ( -12.95952864787948755, -30.95583473709188382, 40.14257249208304756 ) ) ;
#5518 = CARTESIAN_POINT ( 'NONE',  ( -19.41254052147348830, -26.35725562635142083, 34.01367750791696665 ) ) ;
#5519 = CARTESIAN_POINT ( 'NONE',  ( 3.796994071234847710E-16, 61.93301269999999903, 48.95000000109246940 ) ) ;
#5520 = EDGE_CURVE ( 'NONE', #17001, #14616, #12974, .T. ) ;
#5521 = EDGE_CURVE ( 'NONE', #3347, #8366, #2320, .T. ) ;
#5522 = CARTESIAN_POINT ( 'NONE',  ( -18.78091578003892081, -20.46040770435013556, 26.58007249208304401 ) ) ;
#5523 = CARTESIAN_POINT ( 'NONE',  ( 32.50000000000000000, 52.00000000000000711, 15.00000000000000000 ) ) ;
#5524 = ORIENTED_EDGE ( 'NONE', *, *, #2433, .F. ) ;
#5525 = LINE ( 'NONE', #14536, #13899 ) ;
#5526 = CARTESIAN_POINT ( 'NONE',  ( -18.78091578003889950, -27.53959229564985378, 28.54492750791695954 ) ) ;
#5527 = EDGE_CURVE ( 'NONE', #14697, #18570, #17321, .T. ) ;
#5528 = CARTESIAN_POINT ( 'NONE',  ( -41.00000000000000711, 53.00000000000000711, 27.50000000000000000 ) ) ;
#5529 = CIRCLE ( 'NONE', #11459, 7.000000000000004441 ) ;
#5530 = PLANE ( 'NONE',  #1260 ) ;
#5531 = CARTESIAN_POINT ( 'NONE',  ( 37.49999999999999289, 107.3545527679194436, -25.00000000000001421 ) ) ;
#5532 = CARTESIAN_POINT ( 'NONE',  ( -10.58745947852648328, -26.35725562635138530, 34.23632249208304046 ) ) ;
#5533 = AXIS2_PLACEMENT_3D ( 'NONE', #18062, #10589, #18263 ) ;
#5534 = CARTESIAN_POINT ( 'NONE',  ( 2.066987300000002303, 63.14382582708705627, 45.30000000109247082 ) ) ;
#5535 = CARTESIAN_POINT ( 'NONE',  ( 2.066987300000001415, 64.85617417291294373, 48.60000000109246798 ) ) ;
#5536 = EDGE_CURVE ( 'NONE', #18722, #16082, #10240, .T. ) ;
#5537 = LINE ( 'NONE', #13063, #5238 ) ;
#5538 = CARTESIAN_POINT ( 'NONE',  ( -1.461580736456473462, 62.53841926354353120, 45.05000000109246372 ) ) ;
#5539 = LINE ( 'NONE', #17486, #14273 ) ;
#5540 = ORIENTED_EDGE ( 'NONE', *, *, #10084, .F. ) ;
#5541 = EDGE_CURVE ( 'NONE', #17455, #5479, #10134, .T. ) ;
#5542 =( GEOMETRIC_REPRESENTATION_CONTEXT ( 3 ) GLOBAL_UNCERTAINTY_ASSIGNED_CONTEXT ( ( #15907 ) ) GLOBAL_UNIT_ASSIGNED_CONTEXT ( ( #14288, #6747, #18623 ) ) REPRESENTATION_CONTEXT ( 'NONE', 'WORKASPACE' ) );
#5543 =( NAMED_UNIT ( * ) SI_UNIT ( $, .STERADIAN. ) SOLID_ANGLE_UNIT ( ) );
#5544 = CARTESIAN_POINT ( 'NONE',  ( -0.8561741729129461742, 66.06698730000000808, 44.60000000109246798 ) ) ;
#5545 = CARTESIAN_POINT ( 'NONE',  ( -13.82508104294698192, -29.04416526290806644, 6.669927507916955989 ) ) ;
#5546 = CARTESIAN_POINT ( 'NONE',  ( 50.00000000000000000, 3.000000000000000000, -60.00000000000000000 ) ) ;
#5547 = CARTESIAN_POINT ( 'NONE',  ( -20.24501739517669563, -18.99630608921239627, 26.58007249208304046 ) ) ;
#5548 = CARTESIAN_POINT ( 'NONE',  ( -2.066987300000001859, 64.85617417291294373, 48.10000000109246798 ) ) ;
#5549 = EDGE_CURVE ( 'NONE', #15869, #5273, #10281, .T. ) ;
#5550 = DIRECTION ( 'NONE',  ( 0.000000000000000000, 0.000000000000000000, 1.000000000000000000 ) ) ;
#5551 = CARTESIAN_POINT ( 'NONE',  ( 1.767766952966370653, 62.23223304703363112, 45.60000000218494165 ) ) ;
#5552 = CARTESIAN_POINT ( 'NONE',  ( 0.8561741729129471734, 61.93301270000000613, 47.40000000109247225 ) ) ;
#5553 = CARTESIAN_POINT ( 'NONE',  ( 2.500000000000001776, 64.00000000000000000, 49.99999999999999289 ) ) ;
#5554 = FACE_OUTER_BOUND ( 'NONE', #14896, .T. ) ;
#5555 = DIRECTION ( 'NONE',  ( 1.734723475976807094E-15, -1.000000000000000000, 0.000000000000000000 ) ) ;
#5556 = ADVANCED_FACE ( 'NONE', ( #11610 ), #12492, .F. ) ;
#5557 = EDGE_CURVE ( 'NONE', #7381, #16262, #16333, .T. ) ;
#5558 = EDGE_LOOP ( 'NONE', ( #12166, #2577, #12505, #4584 ) ) ;
#5559 = ORIENTED_EDGE ( 'NONE', *, *, #15157, .F. ) ;
#5560 = CARTESIAN_POINT ( 'NONE',  ( -14.83517299489734853, -30.99999999999998224, 8.861322492083038682 ) ) ;
#5561 =( NAMED_UNIT ( * ) SI_UNIT ( $, .STERADIAN. ) SOLID_ANGLE_UNIT ( ) );
#5562 = VERTEX_POINT ( 'NONE', #8677 ) ;
#5564 = ORIENTED_EDGE ( 'NONE', *, *, #5521, .F. ) ;
#5563 = VERTEX_POINT ( 'NONE', #14658 ) ;
#5565 = CARTESIAN_POINT ( 'NONE',  ( -15.96867458239599635, -21.04416526290806999, 42.76757249208304756 ) ) ;
#5566 = EDGE_CURVE ( 'NONE', #13223, #2714, #5297, .T. ) ;
#5567 = CARTESIAN_POINT ( 'NONE',  ( -18.64274437364853654, -29.97976432393976509, 33.57617750791695954 ) ) ;
#5568 = DIRECTION ( 'NONE',  ( 0.000000000000000000, -1.000000000000000000, 0.000000000000000000 ) ) ;
#5569 = CARTESIAN_POINT ( 'NONE',  ( 3.796994071234847710E-16, 61.93301269999999903, 48.95000000109246940 ) ) ;
#5570 = DIRECTION ( 'NONE',  ( 0.000000000000000000, 0.000000000000000000, -1.000000000000000000 ) ) ;
#5571 = ORIENTED_EDGE ( 'NONE', *, *, #18746, .T. ) ;
#5572 = DIRECTION ( 'NONE',  ( 0.000000000000000000, 0.000000000000000000, -1.000000000000000000 ) ) ;
#5573 = EDGE_LOOP ( 'NONE', ( #650, #12370, #14373, #12259 ) ) ;
#5574 = LINE ( 'NONE', #8329, #6886 ) ;
#5575 = ORIENTED_EDGE ( 'NONE', *, *, #11475, .T. ) ;
#5576 = CARTESIAN_POINT ( 'NONE',  ( -0.2730872843520700810, 61.94666219239776694, 45.00000000000001421 ) ) ;
#5577 = PLANE ( 'NONE',  #6853 ) ;
#5578 = CARTESIAN_POINT ( 'NONE',  ( -40.00000000000000711, 113.0000000000000000, -50.00000000000000000 ) ) ;
#5579 = CARTESIAN_POINT ( 'NONE',  ( -1.461580736456473906, 65.46158073645646880, 45.45000000109246940 ) ) ;
#5580 = EDGE_CURVE ( 'NONE', #17240, #2533, #1434, .T. ) ;
#5581 = DIRECTION ( 'NONE',  ( -1.000000000000000000, -0.000000000000000000, -0.000000000000000000 ) ) ;
#5582 = CARTESIAN_POINT ( 'NONE',  ( -2.500000000000001776, 64.00000000000000000, 49.19999999999999574 ) ) ;
#5583 = CARTESIAN_POINT ( 'NONE',  ( 21.50000000000001421, 2.999000000000001442, 32.49999999999998579 ) ) ;
#5584 = ORIENTED_EDGE ( 'NONE', *, *, #4850, .T. ) ;
#5586 = ORIENTED_EDGE ( 'NONE', *, *, #19039, .F. ) ;
#5585 = ORIENTED_EDGE ( 'NONE', *, *, #625, .F. ) ;
#5587 = CARTESIAN_POINT ( 'NONE',  ( -19.41254052147348830, -26.35725562635142083, 39.26367750791695954 ) ) ;
#5588 = VECTOR ( 'NONE', #1337, 1000.000000000000000 ) ;
#5589 = PLANE ( 'NONE',  #4285 ) ;
#5590 = VERTEX_POINT ( 'NONE', #3090 ) ;
#5591 = CARTESIAN_POINT ( 'NONE',  ( -17.68048971390462754, -22.64274437364856496, 10.61132249208304401 ) ) ;
#5592 = LINE ( 'NONE', #17549, #14687 ) ;
#5593 = ORIENTED_EDGE ( 'NONE', *, *, #18394, .T. ) ;
#5594 = CARTESIAN_POINT ( 'NONE',  ( -15.63902057219073605, -27.04416526290807710, 40.58007249208304756 ) ) ;
#5595 = VECTOR ( 'NONE', #14276, 1000.000000000000000 ) ;
#5596 = DIRECTION ( 'NONE',  ( 1.000000000000000000, -0.000000000000000000, -0.000000000000000000 ) ) ;
#5597 = VERTEX_POINT ( 'NONE', #5846 ) ;
#5598 = CARTESIAN_POINT ( 'NONE',  ( 2.500000000000001776, 64.00000000000000000, 46.50000000218494733 ) ) ;
#5599 = ORIENTED_EDGE ( 'NONE', *, *, #19379, .F. ) ;
#5600 = CARTESIAN_POINT ( 'NONE',  ( -50.00000000000002132, 118.0000000000000142, -60.00000000000002132 ) ) ;
#5601 = DIRECTION ( 'NONE',  ( -0.000000000000000000, -1.000000000000000000, -0.000000000000000000 ) ) ;
#5602 = VECTOR ( 'NONE', #134, 1000.000000000000000 ) ;
#5603 = CARTESIAN_POINT ( 'NONE',  ( 2.500000000000010658, 62.96446609406726225, 48.05000000218495160 ) ) ;
#5604 = EDGE_CURVE ( 'NONE', #2159, #12653, #14765, .T. ) ;
#5605 = SHAPE_DEFINITION_REPRESENTATION ( #8792, #15288 ) ;
#5606 = CARTESIAN_POINT ( 'NONE',  ( -1.530808498934192803E-16, 66.50000000000000000, 48.30000000218494449 ) ) ;
#5607 =( BOUNDED_CURVE ( )  B_SPLINE_CURVE ( 2, ( #18203, #2014, #11021, #15544, #15347, #8003, #2114, #5155, #17113 ),
 .UNSPECIFIED., .F., .F. ) 
 B_SPLINE_CURVE_WITH_KNOTS ( ( 3, 2, 2, 2, 3 ),
 ( 0.5000000000000001110, 0.5178571428571430157, 0.5357142857142858094, 0.5535714285714286031, 0.5714285714285713969 ),
 .UNSPECIFIED. ) 
 CURVE ( )  GEOMETRIC_REPRESENTATION_ITEM ( )  RATIONAL_B_SPLINE_CURVE ( ( 0.9999999999999995559, 0.9238795325112871826, 1.000000000000000000, 0.9238795325112867385, 1.000000000000000000, 0.9238795325112867385, 1.000000000000000000, 0.9238795325112867385, 1.000000000000000000 ) ) 
 REPRESENTATION_ITEM ( '' )  );
#5608 = CARTESIAN_POINT ( 'NONE',  ( -17.35725562635144215, -19.58745947852648683, 30.07617750791695599 ) ) ;
#5609 = DIRECTION ( 'NONE',  ( 0.000000000000000000, -0.7893522173763268812, -0.6139406135149196864 ) ) ;
#5610 = CARTESIAN_POINT ( 'NONE',  ( -19.99999999999999645, -23.83517299489738051, 2.951177507916958209 ) ) ;
#5611 = AXIS2_PLACEMENT_3D ( 'NONE', #3928, #17359, #15991 ) ;
#5612 = FACE_OUTER_BOUND ( 'NONE', #2124, .T. ) ;
#5613 = VERTEX_POINT ( 'NONE', #17701 ) ;
#5614 = CARTESIAN_POINT ( 'NONE',  ( -19.24771351637086880, -26.64274437364857206, 9.736322492083042235 ) ) ;
#5615 = VECTOR ( 'NONE', #5038, 1000.000000000000000 ) ;
#5616 = CARTESIAN_POINT ( 'NONE',  ( -11.64274437364854187, -30.14459132904234195, 1.201177507916956433 ) ) ;
#5617 = VECTOR ( 'NONE', #7961, 1000.000000000000000 ) ;
#5618 = CARTESIAN_POINT ( 'NONE',  ( 0.8561741729129460632, 66.06698729999999387, 46.90000000109247225 ) ) ;
#5619 = CARTESIAN_POINT ( 'NONE',  ( -17.51566270880199738, -25.64274437364856496, 4.486322492083042235 ) ) ;
#5620 = CARTESIAN_POINT ( 'NONE',  ( 1.753982408753060440, -45.28611686177728046, 3.000000000000000000 ) ) ;
#5621 = ORIENTED_EDGE ( 'NONE', *, *, #876, .T. ) ;
#5622 = DIRECTION ( 'NONE',  ( 2.665111688417744333E-15, 1.000000000000000000, 0.000000000000000000 ) ) ;
#5623 = CARTESIAN_POINT ( 'NONE',  ( -16.17491895705301275, -18.95583473709189803, 30.29492750791695244 ) ) ;
#5624 = PLANE ( 'NONE',  #14239 ) ;
#5626 = DIRECTION ( 'NONE',  ( -0.000000000000000000, 1.000000000000000000, -0.000000000000000000 ) ) ;
#5625 = VECTOR ( 'NONE', #18935, 1000.000000000000114 ) ;
#5627 = DIRECTION ( 'NONE',  ( 0.1648270051026190508, 0.000000000000000000, -0.9863224920830413467 ) ) ;
#5628 = CARTESIAN_POINT ( 'NONE',  ( -10.75228648362912232, -21.35725562635138530, 33.36132249208304046 ) ) ;
#5629 = CARTESIAN_POINT ( 'NONE',  ( 2.500000000000001776, 64.00000000000000000, 47.99999999999999289 ) ) ;
#5630 = CARTESIAN_POINT ( 'NONE',  ( 0.8561741729129460632, 66.06698730000000808, 49.50000000109246656 ) ) ;
#5631 = VECTOR ( 'NONE', #3193, 1000.000000000000000 ) ;
#5632 = PLANE ( 'NONE',  #17125 ) ;
#5633 = CARTESIAN_POINT ( 'NONE',  ( 0.8561741729129460632, 66.06698729999999387, 45.50000000109247367 ) ) ;
#5634 = DIRECTION ( 'NONE',  ( 0.000000000000000000, 0.000000000000000000, -1.000000000000000000 ) ) ;
#5635 = AXIS2_PLACEMENT_3D ( 'NONE', #14907, #9213, #15106 ) ;
#5636 = EDGE_LOOP ( 'NONE', ( #13367, #3282, #1046, #15658, #6962 ) ) ;
#5637 = CARTESIAN_POINT ( 'NONE',  ( 0.000000000000000000, 0.000000000000000000, 0.000000000000000000 ) ) ;
#5638 = CARTESIAN_POINT ( 'NONE',  ( -20.04416526290808065, -25.17491895705300209, 7.982427507916958653 ) ) ;
#5639 = AXIS2_PLACEMENT_3D ( 'NONE', #939, #1037, #9939 ) ;
#5640 = CARTESIAN_POINT ( 'NONE',  ( -19.41254052147348830, -26.35725562635142083, 7.763677507916958653 ) ) ;
#5641 = CARTESIAN_POINT ( 'NONE',  ( 0.000000000000000000, 0.000000000000000000, 4.500000000000000888 ) ) ;
#5642 = EDGE_CURVE ( 'NONE', #7137, #5957, #19077, .T. ) ;
#5643 = CARTESIAN_POINT ( 'NONE',  ( -15.16482700510264436, -16.99999999999997868, 32.48632249208304046 ) ) ;
#5644 = VECTOR ( 'NONE', #4309, 1000.000000000000000 ) ;
#5645 = CARTESIAN_POINT ( 'NONE',  ( 2.066987300000001415, 64.00000000000000000, 47.75000000109246656 ) ) ;
#5646 = CARTESIAN_POINT ( 'NONE',  ( -15.16482700510260706, -26.99999999999998579, 33.13867750791695954 ) ) ;
#5647 = CARTESIAN_POINT ( 'NONE',  ( -1.035533905932738863, 61.50000000000000000, 45.45000000218494307 ) ) ;
#5648 = COLOUR_RGB ( '', 0.66274510, 0.83137255, 0.94901961) ;
#5649 = CARTESIAN_POINT ( 'NONE',  ( -41.00000000000000711, 53.00000000000000711, -44.00000000000000000 ) ) ;
#5650 = DIRECTION ( 'NONE',  ( 0.000000000000000000, 0.000000000000000000, -1.000000000000000000 ) ) ;
#5651 = CIRCLE ( 'NONE', #9402, 2.500000000000000444 ) ;
#5652 = CARTESIAN_POINT ( 'NONE',  ( -2.066987300000001415, 64.85617417291294373, 47.30000000109247082 ) ) ;
#5653 = CARTESIAN_POINT ( 'NONE',  ( -40.00000000000000711, 110.0000000000000000, 21.00000000000000000 ) ) ;
#5654 = EDGE_CURVE ( 'NONE', #9953, #2052, #8874, .T. ) ;
#5655 = AXIS2_PLACEMENT_3D ( 'NONE', #2325, #1043, #14663 ) ;
#5656 = CARTESIAN_POINT ( 'NONE',  ( 0.000000000000000000, 64.00000000000000000, 45.00000000000000000 ) ) ;
#5657 = VERTEX_POINT ( 'NONE', #14858 ) ;
#5658 = ORIENTED_EDGE ( 'NONE', *, *, #3795, .F. ) ;
#5659 = CARTESIAN_POINT ( 'NONE',  ( -18.35725562635138886, -30.14459132904237393, 9.298822492083038682 ) ) ;
#5660 = ORIENTED_EDGE ( 'NONE', *, *, #11029, .F. ) ;
#5661 = AXIS2_PLACEMENT_3D ( 'NONE', #4003, #691, #5572 ) ;
#5663 = ORIENTED_EDGE ( 'NONE', *, *, #165, .T. ) ;
#5662 = ORIENTED_EDGE ( 'NONE', *, *, #19308, .T. ) ;
#5664 = CARTESIAN_POINT ( 'NONE',  ( -12.31951028609536536, -25.35725562635139596, 39.48632249208304756 ) ) ;
#5665 = CARTESIAN_POINT ( 'NONE',  ( -7.999999999999996447, -24.16482700510256976, 37.07617750791694533 ) ) ;
#5666 = VECTOR ( 'NONE', #17188, 1000.000000000000000 ) ;
#5667 = FACE_OUTER_BOUND ( 'NONE', #1122, .T. ) ;
#5668 = CARTESIAN_POINT ( 'NONE',  ( 2.500000000000001776, 64.00000000000000000, 45.70000000218494307 ) ) ;
#5669 = CARTESIAN_POINT ( 'NONE',  ( -24.00000000000000000, 53.00000000000000711, 20.00000000000000000 ) ) ;
#5670 = VERTEX_POINT ( 'NONE', #11706 ) ;
#5671 = AXIS2_PLACEMENT_3D ( 'NONE', #14430, #1005, #14151 ) ;
#5672 = CARTESIAN_POINT ( 'NONE',  ( 1.035533905932739751, 61.50000000000000000, 46.24999999999999289 ) ) ;
#5673 = ORIENTED_EDGE ( 'NONE', *, *, #14059, .T. ) ;
#5674 = EDGE_CURVE ( 'NONE', #201, #11043, #12003, .T. ) ;
#5675 = ADVANCED_FACE ( 'NONE', ( #10434 ), #19371, .F. ) ;
#5676 = EDGE_LOOP ( 'NONE', ( #13004, #12939, #11992, #12629 ) ) ;
#5677 = DIRECTION ( 'NONE',  ( -0.000000000000000000, -0.000000000000000000, -1.000000000000000000 ) ) ;
#5678 = DIRECTION ( 'NONE',  ( 1.000000000000000000, -0.000000000000000000, 0.000000000000000000 ) ) ;
#5679 = CARTESIAN_POINT ( 'NONE',  ( -10.00000000000000000, 0.000000000000000000, 7.999999999999996447 ) ) ;
#5680 = EDGE_CURVE ( 'NONE', #13683, #2416, #4577, .T. ) ;
#5681 = CIRCLE ( 'NONE', #8808, 1.599999999999997202 ) ;
#5682 = CARTESIAN_POINT ( 'NONE',  ( 0.8561741729129460632, 66.06698729999999387, 49.50000000109246656 ) ) ;
#5683 = PLANE ( 'NONE',  #18798 ) ;
#5684 = AXIS2_PLACEMENT_3D ( 'NONE', #15850, #9768, #12798 ) ;
#5685 = DIRECTION ( 'NONE',  ( 1.156482317317871725E-16, -1.000000000000000000, 0.000000000000000000 ) ) ;
#5686 = FACE_OUTER_BOUND ( 'NONE', #15180, .T. ) ;
#5687 = ORIENTED_EDGE ( 'NONE', *, *, #6658, .T. ) ;
#5689 = VERTEX_POINT ( 'NONE', #10534 ) ;
#5688 = ORIENTED_EDGE ( 'NONE', *, *, #1106, .F. ) ;
#5690 = CARTESIAN_POINT ( 'NONE',  ( -16.17491895705301275, -18.95583473709189803, 40.79492750791695954 ) ) ;
#5691 = AXIS2_PLACEMENT_3D ( 'NONE', #11192, #902, #11290 ) ;
#5692 = CARTESIAN_POINT ( 'NONE',  ( -1.530808498934192803E-16, 66.50000000000000000, 45.00000000000000000 ) ) ;
#5693 = VERTEX_POINT ( 'NONE', #11914 ) ;
#5694 = ORIENTED_EDGE ( 'NONE', *, *, #19018, .F. ) ;
#5695 = CARTESIAN_POINT ( 'NONE',  ( -16.35725562635141372, -26.68048971390461332, 4.048822492083043123 ) ) ;
#5696 = CARTESIAN_POINT ( 'NONE',  ( -2.500000000000006661, 65.03553390593272354, 45.14999999999999858 ) ) ;
#5697 = EDGE_CURVE ( 'NONE', #9017, #17877, #4280, .T. ) ;
#5698 = APPLICATION_CONTEXT ( 'automotive_design' ) ;
#5699 = ADVANCED_FACE ( 'NONE', ( #13184 ), #8863, .T. ) ;
#5700 = VERTEX_POINT ( 'NONE', #14319 ) ;
#5701 = CARTESIAN_POINT ( 'NONE',  ( -13.64274437364856141, -26.68048971390460622, 1.201177507916959986 ) ) ;
#5702 = LINE ( 'NONE', #3932, #17873 ) ;
#5703 = ORIENTED_EDGE ( 'NONE', *, *, #851, .F. ) ;
#5704 = DIRECTION ( 'NONE',  ( 0.000000000000000000, -1.000000000000000000, 0.000000000000000000 ) ) ;
#5705 = ORIENTED_EDGE ( 'NONE', *, *, #6177, .T. ) ;
#5706 = DIRECTION ( 'NONE',  ( -1.000000000000000000, 0.000000000000000000, -0.000000000000000000 ) ) ;
#5707 = DIRECTION ( 'NONE',  ( 0.000000000000000000, 0.000000000000000000, -1.000000000000000000 ) ) ;
#5708 = VECTOR ( 'NONE', #18099, 1000.000000000000000 ) ;
#5709 = CARTESIAN_POINT ( 'NONE',  ( -0.08838834764833032598, 29.80514068711926612, 56.68014068711929809 ) ) ;
#5710 = APPLICATION_PROTOCOL_DEFINITION ( 'draft international standard', 'automotive_design', 1998, #13441 ) ;
#5711 = FACE_OUTER_BOUND ( 'NONE', #8079, .T. ) ;
#5712 = CARTESIAN_POINT ( 'NONE',  ( -15.16482700510259640, -28.99999999999998224, 27.88867750791695954 ) ) ;
#5713 = DIRECTION ( 'NONE',  ( 0.000000000000000000, 0.000000000000000000, -1.000000000000000000 ) ) ;
#5714 = DIRECTION ( 'NONE',  ( 0.000000000000000000, 0.000000000000000000, -1.000000000000000000 ) ) ;
#5715 = DIRECTION ( 'NONE',  ( 0.000000000000000000, -1.000000000000000000, 0.000000000000000000 ) ) ;
#5716 = ORIENTED_EDGE ( 'NONE', *, *, #2886, .T. ) ;
#5717 = CARTESIAN_POINT ( 'NONE',  ( -20.97976432393974022, -27.64274437364858628, 41.23632249208304046 ) ) ;
#5718 = CARTESIAN_POINT ( 'NONE',  ( -9.996306089212364299, -29.24501739517662813, 6.232427507916955989 ) ) ;
#5719 = EDGE_CURVE ( 'NONE', #1836, #9208, #9805, .T. ) ;
#5720 = CARTESIAN_POINT ( 'NONE',  ( 1.461580736456473906, 62.53841926354353120, 45.05000000109246372 ) ) ;
#5721 = CARTESIAN_POINT ( 'NONE',  ( -14.36097942780925685, -20.95583473709189093, 1.205072492083042901 ) ) ;
#5722 = CARTESIAN_POINT ( 'NONE',  ( 1.035533905932739751, 61.50000000000000000, 48.64999999999999858 ) ) ;
#5723 = ORIENTED_EDGE ( 'NONE', *, *, #11548, .F. ) ;
#5724 = FACE_BOUND ( 'NONE', #1216, .T. ) ;
#5725 = CARTESIAN_POINT ( 'NONE',  ( -14.83517299489739649, -18.99999999999997868, 41.01367750791696665 ) ) ;
#5726 = DIRECTION ( 'NONE',  ( -0.000000000000000000, -1.000000000000000000, -0.000000000000000000 ) ) ;
#5727 = DIRECTION ( 'NONE',  ( 0.000000000000000000, 0.000000000000000000, 1.000000000000000000 ) ) ;
#5728 = DIRECTION ( 'NONE',  ( 0.000000000000000000, 0.7071067811865456854, 0.7071067811865494601 ) ) ;
#5729 = CARTESIAN_POINT ( 'NONE',  ( -16.17491895705296656, -29.04416526290807354, 35.33007249208303335 ) ) ;
#5730 = EDGE_CURVE ( 'NONE', #4981, #2835, #16078, .T. ) ;
#5731 = CARTESIAN_POINT ( 'NONE',  ( 4.592425496802577917E-16, 61.50000000000000000, 46.19999999999999574 ) ) ;
#5732 = CARTESIAN_POINT ( 'NONE',  ( -0.8561741729129466183, 61.93301270000000613, 48.30000000109247082 ) ) ;
#5733 = CARTESIAN_POINT ( 'NONE',  ( -5.799326430397251819, 29.65377616443625541, 56.83055285973284754 ) ) ;
#5734 = CARTESIAN_POINT ( 'NONE',  ( 1.035533905932739751, 61.50000000000000000, 45.45000000000000995 ) ) ;
#5735 = CARTESIAN_POINT ( 'NONE',  ( -43.50000000000000000, 118.0000000000000142, 32.50000000000000000 ) ) ;
#5736 = ORIENTED_EDGE ( 'NONE', *, *, #19064, .T. ) ;
#5737 =( NAMED_UNIT ( * ) SI_UNIT ( $, .STERADIAN. ) SOLID_ANGLE_UNIT ( ) );
#5738 = CARTESIAN_POINT ( 'NONE',  ( -19.95583473709191580, -22.49542703274176603, 8.419927507916955989 ) ) ;
#5739 = CARTESIAN_POINT ( 'NONE',  ( -15.96867458239597326, -26.95583473709190159, 38.60742750791696665 ) ) ;
#5740 = DIRECTION ( 'NONE',  ( 0.000000000000000000, -0.000000000000000000, 1.000000000000000000 ) ) ;
#5741 = CARTESIAN_POINT ( 'NONE',  ( -12.64274437364858628, -19.58745947852646552, 1.423822492083040903 ) ) ;
#5742 = CARTESIAN_POINT ( 'NONE',  ( 2.066987300000002303, 63.14382582708705627, 46.90000000109247225 ) ) ;
#5743 = CARTESIAN_POINT ( 'NONE',  ( -9.955834737091912245, -22.82508104294696594, 5.357427507916956877 ) ) ;
#5744 = CARTESIAN_POINT ( 'NONE',  ( -19.95583473709191225, -22.49542703274176603, 8.419927507916954212 ) ) ;
#5745 = CARTESIAN_POINT ( 'NONE',  ( 2.749999999999980460, 115.0000000000000000, 37.49999999999997158 ) ) ;
#5746 = CARTESIAN_POINT ( 'NONE',  ( 44.99999999999997158, 0.000000000000000000, 56.59999999999999432 ) ) ;
#5747 = DIRECTION ( 'NONE',  ( -0.000000000000000000, -0.000000000000000000, -1.000000000000000000 ) ) ;
#5748 = CARTESIAN_POINT ( 'NONE',  ( 0.000000000000000000, 0.000000000000000000, 34.99999999999999289 ) ) ;
#5749 = CARTESIAN_POINT ( 'NONE',  ( -1.461580736456473462, 62.53841926354353120, 47.45000000109246230 ) ) ;
#5750 = FACE_OUTER_BOUND ( 'NONE', #18016, .T. ) ;
#5751 = CARTESIAN_POINT ( 'NONE',  ( -2.500000000000001776, 64.00000000000000000, 44.50000000218494733 ) ) ;
#5752 = ORIENTED_EDGE ( 'NONE', *, *, #2081, .F. ) ;
#5753 = EDGE_LOOP ( 'NONE', ( #7052, #16177 ) ) ;
#5754 = CARTESIAN_POINT ( 'NONE',  ( -18.64274437364860049, -18.02023567606023491, 11.04882249208303868 ) ) ;
#5755 =( LENGTH_UNIT ( ) NAMED_UNIT ( * ) SI_UNIT ( .MILLI., .METRE. ) );
#5756 = CARTESIAN_POINT ( 'NONE',  ( -13.49542703274174116, -28.95583473709188738, 3.392572492083040903 ) ) ;
#5758 = VERTEX_POINT ( 'NONE', #18928 ) ;
#5757 = EDGE_LOOP ( 'NONE', ( #8418, #15963, #18726, #7772, #15025 ) ) ;
#5759 = CARTESIAN_POINT ( 'NONE',  ( -15.16482700510262482, -20.99999999999997513, 42.98632249208304756 ) ) ;
#5760 = CARTESIAN_POINT ( 'NONE',  ( -11.35725562635139418, -29.97976432393972601, 8.423822492083040459 ) ) ;
#5761 = CARTESIAN_POINT ( 'NONE',  ( 0.000000000000000000, 5.051668046482832750E-16, -4.000000000000000000 ) ) ;
#5762 = CARTESIAN_POINT ( 'NONE',  ( -1.265664690411616068E-16, 66.06698730000000808, 49.35000000109246798 ) ) ;
#5763 = VERTEX_POINT ( 'NONE', #17178 ) ;
#5764 = VERTEX_POINT ( 'NONE', #9983 ) ;
#5765 = EDGE_CURVE ( 'NONE', #111, #13544, #712, .T. ) ;
#5766 = ADVANCED_FACE ( 'NONE', ( #19026 ), #18840, .T. ) ;
#5767 = FACE_OUTER_BOUND ( 'NONE', #7732, .T. ) ;
#5768 = ORIENTED_EDGE ( 'NONE', *, *, #14263, .F. ) ;
#5769 = EDGE_LOOP ( 'NONE', ( #15070, #2435, #5913, #1763 ) ) ;
#5770 = CARTESIAN_POINT ( 'NONE',  ( 12.99999999999999822, 0.000000000000000000, 0.000000000000000000 ) ) ;
#5771 = CARTESIAN_POINT ( 'NONE',  ( -1.464522546803548496E-16, 66.39174682499999847, 44.93750000027311842 ) ) ;
#5772 = PLANE ( 'NONE',  #6256 ) ;
#5773 = EDGE_CURVE ( 'NONE', #13043, #11279, #15799, .T. ) ;
#5774 = CARTESIAN_POINT ( 'NONE',  ( -2.066987300000001859, 64.85617417291294373, 46.50000000109246656 ) ) ;
#5775 = DIRECTION ( 'NONE',  ( 0.000000000000000000, 0.000000000000000000, 1.000000000000000000 ) ) ;
#5776 = FACE_OUTER_BOUND ( 'NONE', #3168, .T. ) ;
#5777 = CARTESIAN_POINT ( 'NONE',  ( 2.500000000000001776, 64.00000000000000000, 49.99999999999999289 ) ) ;
#5778 = EDGE_LOOP ( 'NONE', ( #1076, #16702, #4893, #5232 ) ) ;
#5780 = ORIENTED_EDGE ( 'NONE', *, *, #18854, .T. ) ;
#5779 = ORIENTED_EDGE ( 'NONE', *, *, #7396, .T. ) ;
#5781 = CARTESIAN_POINT ( 'NONE',  ( -9.754982604823348780, -18.99630608921234654, -0.3300724920830435116 ) ) ;
#5782 = DIRECTION ( 'NONE',  ( -1.000000000000000000, -0.000000000000000000, -0.000000000000000000 ) ) ;
#5783 = VERTEX_POINT ( 'NONE', #15889 ) ;
#5784 = ADVANCED_FACE ( 'NONE', ( #14414 ), #11461, .F. ) ;
#5785 = VECTOR ( 'NONE', #9246, 1000.000000000000000 ) ;
#5786 = VERTEX_POINT ( 'NONE', #889 ) ;
#5787 = CARTESIAN_POINT ( 'NONE',  ( -14.36097942780925685, -20.95583473709189093, 1.205072492083042901 ) ) ;
#5788 = EDGE_CURVE ( 'NONE', #16741, #2080, #8814, .T. ) ;
#5789 = EDGE_CURVE ( 'NONE', #2227, #587, #5592, .T. ) ;
#5790 = LINE ( 'NONE', #8916, #13123 ) ;
#5791 = ORIENTED_EDGE ( 'NONE', *, *, #8655, .F. ) ;
#5792 = CARTESIAN_POINT ( 'NONE',  ( -14.03132541760401786, -21.04416526290806289, -0.7675724920830402365 ) ) ;
#5793 = CARTESIAN_POINT ( 'NONE',  ( -41.00000000000000711, 110.0000000000000000, -19.00000000000000000 ) ) ;
#5794 = ORIENTED_EDGE ( 'NONE', *, *, #9280, .T. ) ;
#5795 = CARTESIAN_POINT ( 'NONE',  ( -50.00000000000002132, 118.0000000000000142, -60.00000000000002132 ) ) ;
#5796 = ORIENTED_EDGE ( 'NONE', *, *, #16365, .T. ) ;
#5797 = FACE_OUTER_BOUND ( 'NONE', #14917, .T. ) ;
#5798 = CARTESIAN_POINT ( 'NONE',  ( 5.421010862427523748E-15, -25.00000000000000711, 1.500000000000000000 ) ) ;
#5799 = CARTESIAN_POINT ( 'NONE',  ( -41.00000000000000711, 53.00000000000000711, -38.50000000000000711 ) ) ;
#5800 = AXIS2_PLACEMENT_3D ( 'NONE', #7962, #4927, #17074 ) ;
#5801 = PRODUCT_CONTEXT ( 'NONE', #9697, 'mechanical' ) ;
#5802 = FACE_OUTER_BOUND ( 'NONE', #7227, .T. ) ;
#5803 = CARTESIAN_POINT ( 'NONE',  ( -16.17491895705301275, -18.95583473709189803, 25.04492750791695954 ) ) ;
#5804 = CARTESIAN_POINT ( 'NONE',  ( -17.35725562635144215, -19.58745947852648683, 9.076177507916957765 ) ) ;
#5805 = DIRECTION ( 'NONE',  ( 0.000000000000000000, 0.000000000000000000, -1.000000000000000000 ) ) ;
#5806 = EDGE_CURVE ( 'NONE', #15519, #16834, #4131, .T. ) ;
#5807 = ORIENTED_EDGE ( 'NONE', *, *, #3607, .T. ) ;
#5808 = EDGE_CURVE ( 'NONE', #16539, #2289, #798, .T. ) ;
#5809 = CARTESIAN_POINT ( 'NONE',  ( -9.754982604823302594, -29.00369391078756465, 39.70507249208304046 ) ) ;
#5810 = CIRCLE ( 'NONE', #16782, 2.700000000000000622 ) ;
#5811 = CARTESIAN_POINT ( 'NONE',  ( -18.35725562635144925, -17.85540867095761186, 9.076177507916954212 ) ) ;
#5812 = AXIS2_PLACEMENT_3D ( 'NONE', #10451, #1743, #16350 ) ;
#5813 = CARTESIAN_POINT ( 'NONE',  ( 0.08332044287238019042, 25.64046917798804515, 60.84354269072931487 ) ) ;
#5814 = EDGE_CURVE ( 'NONE', #12801, #9275, #14079, .T. ) ;
#5815 = CARTESIAN_POINT ( 'NONE',  ( -13.64274437364857739, -21.31951028609534760, 6.673822492083044011 ) ) ;
#5816 = PLANE ( 'NONE',  #6607 ) ;
#5817 = ORIENTED_EDGE ( 'NONE', *, *, #9803, .F. ) ;
#5818 = CARTESIAN_POINT ( 'NONE',  ( -10.65656631922262321, -20.29120037471566462, 3.747711961066792630E-16 ) ) ;
#5819 = ORIENTED_EDGE ( 'NONE', *, *, #2657, .F. ) ;
#5820 = CARTESIAN_POINT ( 'NONE',  ( -19.99999999999999645, -23.83517299489738051, 39.70117750791695954 ) ) ;
#5821 = DIRECTION ( 'NONE',  ( 0.000000000000000000, -1.000000000000000000, 1.026972870230479989E-15 ) ) ;
#5822 = CARTESIAN_POINT ( 'NONE',  ( -41.00000000000000711, 53.00000000000000711, -37.50000000000000711 ) ) ;
#5823 = FACE_BOUND ( 'NONE', #12544, .T. ) ;
#5824 = DIRECTION ( 'NONE',  ( -0.000000000000000000, -0.000000000000000000, -1.000000000000000000 ) ) ;
#5825 = CARTESIAN_POINT ( 'NONE',  ( 1.035533905932739751, 61.50000000000000000, 47.04999999999999005 ) ) ;
#5826 = CARTESIAN_POINT ( 'NONE',  ( -1.461580736456473462, 62.53841926354353120, 46.65000000109247225 ) ) ;
#5827 = AXIS2_PLACEMENT_3D ( 'NONE', #14664, #14867, #2805 ) ;
#5828 = VECTOR ( 'NONE', #4955, 1000.000000000000000 ) ;
#5829 = PRODUCT_DEFINITION_SHAPE ( 'NONE', 'NONE',  #16256 ) ;
#5830 = ADVANCED_FACE ( 'NONE', ( #5990, #7259 ), #12051, .F. ) ;
#5831 = LINE ( 'NONE', #14746, #2323 ) ;
#5832 = CARTESIAN_POINT ( 'NONE',  ( 2.500000000000001776, 65.03553390593273775, 47.24999999999999289 ) ) ;
#5833 = CARTESIAN_POINT ( 'NONE',  ( -41.00000000000000711, 110.0000000000000000, 14.50000000000000000 ) ) ;
#5834 = ORIENTED_EDGE ( 'NONE', *, *, #5139, .F. ) ;
#5835 = CARTESIAN_POINT ( 'NONE',  ( -20.04416526290808065, -25.17491895705300209, 2.732427507916957765 ) ) ;
#5836 = CARTESIAN_POINT ( 'NONE',  ( -19.24771351637089367, -21.35725562635142438, 8.638677507916957765 ) ) ;
#5837 = CARTESIAN_POINT ( 'NONE',  ( 1.035533905932739751, 61.50000000000000000, 48.75000000218494023 ) ) ;
#5838 = CARTESIAN_POINT ( 'NONE',  ( -17.35725562635140307, -28.41254052147349185, 4.048822492083041347 ) ) ;
#5839 = AXIS2_PLACEMENT_3D ( 'NONE', #11972, #10595, #8733 ) ;
#5840 = AXIS2_PLACEMENT_3D ( 'NONE', #6516, #14242, #5047 ) ;
#5841 = CARTESIAN_POINT ( 'NONE',  ( -1.265664690411616068E-16, 66.06698730000000808, 44.75000000109247367 ) ) ;
#5842 = CARTESIAN_POINT ( 'NONE',  ( -17.64274437364855430, -28.24771351637087236, 2.076177507916958209 ) ) ;
#5843 = PRODUCT_RELATED_PRODUCT_CATEGORY ( 'part', '', ( #18808 ) ) ;
#5844 = CARTESIAN_POINT ( 'NONE',  ( -11.21908421996108984, -20.46040770435011069, 10.16992750791695599 ) ) ;
#5845 = DIRECTION ( 'NONE',  ( -1.000000000000000000, -0.000000000000000000, -0.000000000000000000 ) ) ;
#5846 = CARTESIAN_POINT ( 'NONE',  ( -25.00000000000000711, 110.0000000000000000, 20.00000000000000000 ) ) ;
#5847 = LINE ( 'NONE', #5944, #17791 ) ;
#5848 = CARTESIAN_POINT ( 'NONE',  ( -7.499999999999994671, -38.00000000000000000, 12.50000000000000000 ) ) ;
#5849 = CARTESIAN_POINT ( 'NONE',  ( -24.00000000000000000, 47.00000000000000711, 18.00000000000000355 ) ) ;
#5850 = LINE ( 'NONE', #18008, #14427 ) ;
#5851 =( GEOMETRIC_REPRESENTATION_CONTEXT ( 3 ) GLOBAL_UNCERTAINTY_ASSIGNED_CONTEXT ( ( #14154 ) ) GLOBAL_UNIT_ASSIGNED_CONTEXT ( ( #15196, #1766, #6471 ) ) REPRESENTATION_CONTEXT ( 'NONE', 'WORKASPACE' ) );
#5852 = VECTOR ( 'NONE', #17395, 1000.000000000000000 ) ;
#5853 = DIRECTION ( 'NONE',  ( 1.000000000000000000, -0.000000000000000000, -0.000000000000000000 ) ) ;
#5854 = ORIENTED_EDGE ( 'NONE', *, *, #14798, .F. ) ;
#5855 = ORIENTED_EDGE ( 'NONE', *, *, #12708, .F. ) ;
#5856 = CARTESIAN_POINT ( 'NONE',  ( -12.95952864787948755, -30.95583473709188382, 13.89257249208304046 ) ) ;
#5857 =( NAMED_UNIT ( * ) PLANE_ANGLE_UNIT ( ) SI_UNIT ( $, .RADIAN. ) );
#5858 = CARTESIAN_POINT ( 'NONE',  ( 2.500000000000001776, 64.00000000000000000, 47.19999999999999574 ) ) ;
#5860 = ORIENTED_EDGE ( 'NONE', *, *, #4091, .F. ) ;
#5859 = ORIENTED_EDGE ( 'NONE', *, *, #1853, .F. ) ;
#5861 = CARTESIAN_POINT ( 'NONE',  ( -17.68048971390461688, -25.35725562635141372, 18.26367750791696309 ) ) ;
#5862 = DIRECTION ( 'NONE',  ( -1.541976423090495633E-16, 0.000000000000000000, 1.000000000000000000 ) ) ;
#5863 = CARTESIAN_POINT ( 'NONE',  ( -9.996306089212408708, -18.75498260482328661, 1.642572492083039126 ) ) ;
#5864 = CARTESIAN_POINT ( 'NONE',  ( -25.00000000000000000, 113.0000000000000000, 30.00000000000000000 ) ) ;
#5865 = CARTESIAN_POINT ( 'NONE',  ( -2.500000000000001776, 64.00000000000000000, 45.30000000218493739 ) ) ;
#5866 = ORIENTED_EDGE ( 'NONE', *, *, #15046, .T. ) ;
#5867 = ORIENTED_EDGE ( 'NONE', *, *, #6958, .F. ) ;
#5868 = CARTESIAN_POINT ( 'NONE',  ( -1.767766952966369765, 62.23223304703363112, 46.89999999999999858 ) ) ;
#5869 = DIRECTION ( 'NONE',  ( 0.000000000000000000, -0.7071067811865493491, 0.7071067811865457964 ) ) ;
#5870 = ORIENTED_EDGE ( 'NONE', *, *, #15643, .F. ) ;
#5871 = LINE ( 'NONE', #18030, #9675 ) ;
#5872 = LINE ( 'NONE', #10562, #4692 ) ;
#5873 = CARTESIAN_POINT ( 'NONE',  ( -0.8561741729129465073, 61.93301270000000613, 49.10000000109246088 ) ) ;
#5874 = DIRECTION ( 'NONE',  ( 0.000000000000000000, 0.7071067811865456854, 0.7071067811865494601 ) ) ;
#5875 = PLANE ( 'NONE',  #18021 ) ;
#5876 = ORIENTED_EDGE ( 'NONE', *, *, #4751, .F. ) ;
#5878 = VERTEX_POINT ( 'NONE', #1378 ) ;
#5877 = EDGE_LOOP ( 'NONE', ( #14602, #15858, #10852, #7263, #3734 ) ) ;
#5879 = ADVANCED_FACE ( 'NONE', ( #17648 ), #16377, .T. ) ;
#5881 = EDGE_CURVE ( 'NONE', #5758, #18462, #15001, .T. ) ;
#5880 = CARTESIAN_POINT ( 'NONE',  ( -7.999999999999996447, -24.16482700510256976, 21.32617750791695599 ) ) ;
#5882 = CARTESIAN_POINT ( 'NONE',  ( -1.530808498934192803E-16, 66.50000000000000000, 45.00000000000000000 ) ) ;
#5883 = ORIENTED_EDGE ( 'NONE', *, *, #620, .T. ) ;
#5884 = EDGE_LOOP ( 'NONE', ( #3569, #4514, #13419, #7979 ) ) ;
#5885 = CARTESIAN_POINT ( 'NONE',  ( -13.49542703274174116, -28.95583473709188738, 40.14257249208304756 ) ) ;
#5886 = EDGE_CURVE ( 'NONE', #14875, #10285, #3, .T. ) ;
#5887 = DIRECTION ( 'NONE',  ( -1.541976423090495880E-16, 0.000000000000000000, 1.000000000000000000 ) ) ;
#5888 = DIRECTION ( 'NONE',  ( -2.081668171172167774E-16, 0.000000000000000000, 1.000000000000000000 ) ) ;
#5889 = ORIENTED_EDGE ( 'NONE', *, *, #16114, .F. ) ;
#5890 = CARTESIAN_POINT ( 'NONE',  ( -12.04416526290807887, -24.96867458239596260, 0.5449275079169599856 ) ) ;
#5891 = EDGE_CURVE ( 'NONE', #18739, #5079, #17948, .T. ) ;
#5892 = CARTESIAN_POINT ( 'NONE',  ( -2.500000000000011546, 65.03553390593272354, 44.45000000218495018 ) ) ;
#5893 = ORIENTED_EDGE ( 'NONE', *, *, #500, .F. ) ;
#5894 = CARTESIAN_POINT ( 'NONE',  ( 1.300000000000000044, -0.7390083445627200209, 1.280000000000001137 ) ) ;
#5895 = ORIENTED_EDGE ( 'NONE', *, *, #10385, .F. ) ;
#5896 = CARTESIAN_POINT ( 'NONE',  ( -31.74999999999995737, 3.061616997868383634E-16, -2.500000000000000444 ) ) ;
#5897 = DIRECTION ( 'NONE',  ( -0.000000000000000000, -0.000000000000000000, -1.000000000000000000 ) ) ;
#5898 = CARTESIAN_POINT ( 'NONE',  ( -32.50000000000002132, 0.000000000000000000, -25.00000000000002842 ) ) ;
#5899 = PRODUCT_CONTEXT ( 'NONE', #2313, 'mechanical' ) ;
#5900 = CYLINDRICAL_SURFACE ( 'NONE', #2557, 1.599999999999997202 ) ;
#5901 = VECTOR ( 'NONE', #14960, 1000.000000000000000 ) ;
#5902 = CARTESIAN_POINT ( 'NONE',  ( 1.035533905932738197, 66.50000000000000000, 48.14999999999999858 ) ) ;
#5903 = CARTESIAN_POINT ( 'NONE',  ( 2.492551403682577771, 31.20336399182262710, 54.92836399182266405 ) ) ;
#5904 = CARTESIAN_POINT ( 'NONE',  ( -24.00000000000000000, 110.0000000000000000, 30.00000000000000000 ) ) ;
#5905 = LINE ( 'NONE', #13438, #11771 ) ;
#5906 = ORIENTED_EDGE ( 'NONE', *, *, #15756, .F. ) ;
#5907 = CARTESIAN_POINT ( 'NONE',  ( -16.50457296725825174, -19.04416526290807354, 6.017572492083042235 ) ) ;
#5908 = CARTESIAN_POINT ( 'NONE',  ( -9.754982604823348780, -18.99630608921234654, 4.919927507916955989 ) ) ;
#5909 = CARTESIAN_POINT ( 'NONE',  ( 2.500000000000001776, 64.00000000000000000, 48.10000000218494165 ) ) ;
#5910 = CARTESIAN_POINT ( 'NONE',  ( -12.68318583509882380, -26.07549068051207541, 8.205072492083042235 ) ) ;
#5911 = AXIS2_PLACEMENT_3D ( 'NONE', #3580, #251, #5065 ) ;
#5912 = DIRECTION ( 'NONE',  ( -1.000000000000000000, 0.000000000000000000, -0.000000000000000000 ) ) ;
#5913 = ORIENTED_EDGE ( 'NONE', *, *, #5281, .T. ) ;
#5914 = CARTESIAN_POINT ( 'NONE',  ( 20.00000000000000355, 0.000000000000000000, 0.000000000000000000 ) ) ;
#5915 = VERTEX_POINT ( 'NONE', #16271 ) ;
#5916 = CARTESIAN_POINT ( 'NONE',  ( -10.00000000000000000, -37.50000000000000000, 7.999999999999996447 ) ) ;
#5917 = CARTESIAN_POINT ( 'NONE',  ( 44.99999999999997158, 3.000000000000000000, 56.59999999999999432 ) ) ;
#5918 = LINE ( 'NONE', #2877, #10288 ) ;
#5919 = PLANE ( 'NONE',  #18193 ) ;
#5920 = EDGE_CURVE ( 'NONE', #9490, #12155, #11957, .T. ) ;
#5921 = EDGE_CURVE ( 'NONE', #7863, #13130, #19220, .T. ) ;
#5922 = CARTESIAN_POINT ( 'NONE',  ( -0.8561741729129466183, 61.93301270000000613, 45.90000000109247225 ) ) ;
#5923 = EDGE_CURVE ( 'NONE', #8404, #4643, #18049, .T. ) ;
#5924 = AXIS2_PLACEMENT_3D ( 'NONE', #15186, #16754, #16953 ) ;
#5925 = FACE_OUTER_BOUND ( 'NONE', #9365, .T. ) ;
#5926 = CARTESIAN_POINT ( 'NONE',  ( -1.035533905932738863, 61.50000000000000000, 47.74999999999999289 ) ) ;
#5927 = CARTESIAN_POINT ( 'NONE',  ( -41.00000000000000711, 53.00000000000000711, 6.999999999999999112 ) ) ;
#5928 = VERTEX_POINT ( 'NONE', #10577 ) ;
#5929 = CARTESIAN_POINT ( 'NONE',  ( -17.35725562635144215, -19.58745947852648683, 9.076177507916957765 ) ) ;
#5930 = CARTESIAN_POINT ( 'NONE',  ( -19.24771351637089367, -21.35725562635142438, 13.88867750791695954 ) ) ;
#5931 = CARTESIAN_POINT ( 'NONE',  ( -1.633339126078534154, 65.67088701091057601, 44.99999999999999289 ) ) ;
#5932 = CARTESIAN_POINT ( 'NONE',  ( -11.46040770435014977, -20.21908421996103655, 1.642572492083041125 ) ) ;
#5933 = VECTOR ( 'NONE', #13417, 1000.000000000000000 ) ;
#5934 = DIRECTION ( 'NONE',  ( 1.156482317317871725E-16, 0.000000000000000000, -1.000000000000000000 ) ) ;
#5935 = EDGE_CURVE ( 'NONE', #9405, #12335, #13124, .T. ) ;
#5936 = CARTESIAN_POINT ( 'NONE',  ( -18.53959229564986799, -20.21908421996107563, 8.857427507916957765 ) ) ;
#5937 = EDGE_CURVE ( 'NONE', #12231, #11751, #19124, .T. ) ;
#5938 = DIRECTION ( 'NONE',  ( 1.000000000000000000, 0.000000000000000000, 0.000000000000000000 ) ) ;
#5939 = CARTESIAN_POINT ( 'NONE',  ( -18.53959229564986799, -20.21908421996107563, 8.857427507916957765 ) ) ;
#5940 = VECTOR ( 'NONE', #11369, 1000.000000000000000 ) ;
#5941 = DIRECTION ( 'NONE',  ( -2.775557561562890858E-16, 0.7071067811865456854, 0.7071067811865493491 ) ) ;
#5942 = VECTOR ( 'NONE', #17632, 1000.000000000000000 ) ;
#5943 = DIRECTION ( 'NONE',  ( 0.000000000000000000, 0.000000000000000000, 1.000000000000000000 ) ) ;
#5944 = CARTESIAN_POINT ( 'NONE',  ( -40.00000000000000711, 113.0000000000000000, 0.5000000000000004441 ) ) ;
#5945 = FACE_OUTER_BOUND ( 'NONE', #7066, .T. ) ;
#5946 = VECTOR ( 'NONE', #4722, 1000.000000000000000 ) ;
#5947 = CARTESIAN_POINT ( 'NONE',  ( -2.066987300000000971, 63.14382582708704916, 45.80000000109246372 ) ) ;
#5948 = DIRECTION ( 'NONE',  ( 0.000000000000000000, 0.000000000000000000, 1.000000000000000000 ) ) ;
#5949 = CIRCLE ( 'NONE', #18183, 5.800000000000007816 ) ;
#5950 = PLANE ( 'NONE',  #18036 ) ;
#5951 = ORIENTED_EDGE ( 'NONE', *, *, #9014, .F. ) ;
#5952 = ORIENTED_EDGE ( 'NONE', *, *, #12623, .F. ) ;
#5953 = CARTESIAN_POINT ( 'NONE',  ( -7.955834737091903364, -25.71081734191518464, 13.01757249208304046 ) ) ;
#5954 = CIRCLE ( 'NONE', #7191, 1.678500596222258556 ) ;
#5955 =( NAMED_UNIT ( * ) SI_UNIT ( $, .STERADIAN. ) SOLID_ANGLE_UNIT ( ) );
#5956 = CARTESIAN_POINT ( 'NONE',  ( -41.00000000000000711, 53.00000000000000711, 13.50000000000000000 ) ) ;
#5958 = VERTEX_POINT ( 'NONE', #1578 ) ;
#5957 = VERTEX_POINT ( 'NONE', #10383 ) ;
#5959 = CARTESIAN_POINT ( 'NONE',  ( -12.48433729119798130, -25.64274437364855075, 21.76367750791695954 ) ) ;
#5960 = CARTESIAN_POINT ( 'NONE',  ( -40.00000000000000711, 110.0000000000000000, 30.00000000000000000 ) ) ;
#5961 = CARTESIAN_POINT ( 'NONE',  ( -21.14459132904239169, -20.64274437364858628, 10.61132249208303868 ) ) ;
#5962 = AXIS2_PLACEMENT_3D ( 'NONE', #5523, #11042, #6551 ) ;
#5963 = CARTESIAN_POINT ( 'NONE',  ( -1.265664690411616068E-16, 66.06698730000000808, 44.75000000109247367 ) ) ;
#5964 = CARTESIAN_POINT ( 'NONE',  ( 1.767766952966370653, 62.23223304703363112, 44.80000000218493739 ) ) ;
#5965 = ORIENTED_EDGE ( 'NONE', *, *, #6399, .F. ) ;
#5966 = EDGE_CURVE ( 'NONE', #15107, #15565, #5790, .T. ) ;
#5967 = VERTEX_POINT ( 'NONE', #14906 ) ;
#5968 = CARTESIAN_POINT ( 'NONE',  ( 2.500000000000001776, 64.00000000000000000, 46.39999999999999858 ) ) ;
#5969 = VERTEX_POINT ( 'NONE', #10479 ) ;
#5970 = AXIS2_PLACEMENT_3D ( 'NONE', #8633, #7267, #5706 ) ;
#5971 = ORIENTED_EDGE ( 'NONE', *, *, #15317, .F. ) ;
#5972 = CARTESIAN_POINT ( 'NONE',  ( -10.42301891655615087, -22.26810260968755983, 4.401948939463558987E-14 ) ) ;
#5973 = DIRECTION ( 'NONE',  ( -0.000000000000000000, -0.000000000000000000, -1.000000000000000000 ) ) ;
#5974 = AXIS2_PLACEMENT_3D ( 'NONE', #19307, #17834, #13513 ) ;
#5975 = CARTESIAN_POINT ( 'NONE',  ( 1.461580736456473684, 65.46158073645646880, 47.05000000109247082 ) ) ;
#5976 = CARTESIAN_POINT ( 'NONE',  ( -25.00000000000000000, 110.0000000000000000, 8.000000000000000000 ) ) ;
#5977 = STYLED_ITEM ( 'NONE', ( #1872 ), #4051 ) ;
#5978 = DIRECTION ( 'NONE',  ( 0.000000000000000000, 0.8660254037844380415, -0.5000000000000011102 ) ) ;
#5979 = ORIENTED_EDGE ( 'NONE', *, *, #15135, .F. ) ;
#5981 = EDGE_LOOP ( 'NONE', ( #8881, #8921, #9288, #14834 ) ) ;
#5980 = ORIENTED_EDGE ( 'NONE', *, *, #4698, .T. ) ;
#5982 = CARTESIAN_POINT ( 'NONE',  ( -21.95583473709191580, -21.95952864787954084, 18.91992750791695954 ) ) ;
#5983 = CARTESIAN_POINT ( 'NONE',  ( 11.83926609531033058, -43.78611686177728046, 3.000000000000000000 ) ) ;
#5984 = VECTOR ( 'NONE', #3051, 1000.000000000000000 ) ;
#5985 = ORIENTED_EDGE ( 'NONE', *, *, #11656, .F. ) ;
#5986 = ORIENTED_EDGE ( 'NONE', *, *, #3297, .T. ) ;
#5987 = CARTESIAN_POINT ( 'NONE',  ( -13.35725562635141195, -26.51566270880198672, 24.17382249208304046 ) ) ;
#5988 = AXIS2_PLACEMENT_3D ( 'NONE', #14865, #13382, #11919 ) ;
#5989 = EDGE_CURVE ( 'NONE', #11742, #16466, #16472, .T. ) ;
#5990 = FACE_BOUND ( 'NONE', #854, .T. ) ;
#5991 = CARTESIAN_POINT ( 'NONE',  ( 1.035533905932739751, 61.50000000000000000, 47.15000000218494591 ) ) ;
#5992 = EDGE_CURVE ( 'NONE', #6167, #9683, #2744, .T. ) ;
#5993 = ORIENTED_EDGE ( 'NONE', *, *, #2893, .T. ) ;
#5994 = CARTESIAN_POINT ( 'NONE',  ( -13.64274437364856141, -26.68048971390460622, 6.451177507916961318 ) ) ;
#5995 = CYLINDRICAL_SURFACE ( 'NONE', #19129, 6.799999999999997158 ) ;
#5996 = ORIENTED_EDGE ( 'NONE', *, *, #9440, .F. ) ;
#5997 = DIRECTION ( 'NONE',  ( 1.000000000000000000, 0.000000000000000000, -5.782411586589357392E-17 ) ) ;
#5998 = PRODUCT ( 'Stainless Steel Outer Casing', 'Stainless Steel Outer Casing', '', ( #17564 ) ) ;
#5999 = EDGE_LOOP ( 'NONE', ( #12053, #10256, #5426, #5497, #13808 ) ) ;
#6000 = PLANE ( 'NONE',  #13799 ) ;
#6001 = DIRECTION ( 'NONE',  ( 7.304098846218135653E-17, 0.000000000000000000, -1.000000000000000000 ) ) ;
#6002 = DIRECTION ( 'NONE',  ( 0.000000000000000000, 0.000000000000000000, 1.000000000000000000 ) ) ;
#6003 = VECTOR ( 'NONE', #16284, 1000.000000000000000 ) ;
#6004 = APPLICATION_PROTOCOL_DEFINITION ( 'draft international standard', 'automotive_design', 1998, #5698 ) ;
#6005 = CARTESIAN_POINT ( 'NONE',  ( -32.50000000000000000, 53.00000000000000711, 15.00000000000000000 ) ) ;
#6006 = VECTOR ( 'NONE', #15782, 1000.000000000000000 ) ;
#6007 = CARTESIAN_POINT ( 'NONE',  ( -2.500000000000001776, 65.03553390593273775, 49.94999999999998863 ) ) ;
#6008 = DIRECTION ( 'NONE',  ( 1.000000000000000000, 0.000000000000000000, 0.000000000000000000 ) ) ;
#6009 = CARTESIAN_POINT ( 'NONE',  ( -19.24771351637089367, -21.35725562635142438, 19.13867750791695954 ) ) ;
#6010 = PLANE ( 'NONE',  #3651 ) ;
#6011 = ORIENTED_EDGE ( 'NONE', *, *, #7360, .T. ) ;
#6012 = CARTESIAN_POINT ( 'NONE',  ( -16.50457296725825174, -19.04416526290807354, 21.76757249208304401 ) ) ;
#6013 = EDGE_CURVE ( 'NONE', #5200, #2690, #8716, .T. ) ;
#6014 = CIRCLE ( 'NONE', #5084, 2.649999999999985700 ) ;
#6015 = CARTESIAN_POINT ( 'NONE',  ( -2.500000000000011102, 62.96446609406727646, 47.75000000218493312 ) ) ;
#6016 = B_SPLINE_CURVE_WITH_KNOTS ( 'NONE', 3,
 ( #10726, #17797, #16328, #2895 ),
 .UNSPECIFIED., .F., .F.,
 ( 4, 4 ),
 ( 0.000000000000000000, 1.000000000000000000 ),
 .UNSPECIFIED. ) ;
#6017 = CARTESIAN_POINT ( 'NONE',  ( -17.95583473709190869, -24.96867458239598037, 9.955072492083044011 ) ) ;
#6018 = AXIS2_PLACEMENT_3D ( 'NONE', #2817, #2720, #11724 ) ;
#6019 = LINE ( 'NONE', #9044, #15044 ) ;
#6020 = ORIENTED_EDGE ( 'NONE', *, *, #387, .F. ) ;
#6021 = CARTESIAN_POINT ( 'NONE',  ( -7.499999999999994671, -26.00000000000000355, 9.500000000000001776 ) ) ;
#6022 = ORIENTED_EDGE ( 'NONE', *, *, #15854, .F. ) ;
#6023 = PLANE ( 'NONE',  #10295 ) ;
#6024 = EDGE_CURVE ( 'NONE', #11249, #10297, #17749, .T. ) ;
#6025 = DIRECTION ( 'NONE',  ( 0.000000000000000000, -1.000000000000000000, 0.000000000000000000 ) ) ;
#6026 = CARTESIAN_POINT ( 'NONE',  ( 37.49999999999999289, -6.000000000000000000, 24.99999999999998579 ) ) ;
#6027 = FACE_OUTER_BOUND ( 'NONE', #4822, .T. ) ;
#6028 = CARTESIAN_POINT ( 'NONE',  ( 2.066987300000001415, 64.85617417291294373, 45.40000000109247225 ) ) ;
#6029 = DIRECTION ( 'NONE',  ( 0.000000000000000000, 1.000000000000000000, 0.000000000000000000 ) ) ;
#6030 = CARTESIAN_POINT ( 'NONE',  ( -2.500000000000000888, 62.96446609406726935, 46.04999999999999005 ) ) ;
#6031 = CARTESIAN_POINT ( 'NONE',  ( -41.00000000000000711, 53.00000000000000711, -32.00000000000000000 ) ) ;
#6032 = ORIENTED_EDGE ( 'NONE', *, *, #15148, .F. ) ;
#6033 = CARTESIAN_POINT ( 'NONE',  ( -45.00000000000000000, -3.000000000000002665, 54.99999999999998579 ) ) ;
#6034 = PLANE ( 'NONE',  #4370 ) ;
#6035 = EDGE_CURVE ( 'NONE', #2469, #19221, #1495, .T. ) ;
#6036 = VECTOR ( 'NONE', #9291, 1000.000000000000000 ) ;
#6037 = CARTESIAN_POINT ( 'NONE',  ( -19.99999999999999645, -23.83517299489738051, 13.45117750791695777 ) ) ;
#6038 = CARTESIAN_POINT ( 'NONE',  ( 2.500000000000002220, 62.96446609406726935, 48.85000000218494165 ) ) ;
#6039 = ADVANCED_FACE ( 'NONE', ( #4223 ), #18440, .F. ) ;
#6040 = CARTESIAN_POINT ( 'NONE',  ( -19.95583473709190514, -25.50457296725822687, 9.955072492083036906 ) ) ;
#6041 = CARTESIAN_POINT ( 'NONE',  ( -0.8561741729129461742, 66.06698729999999387, 44.80000000109246372 ) ) ;
#6042 = CARTESIAN_POINT ( 'NONE',  ( -13.82508104294698192, -29.04416526290806644, 6.669927507916955989 ) ) ;
#6043 = DIRECTION ( 'NONE',  ( -1.000000000000000000, -2.312964634635742957E-16, 0.000000000000000000 ) ) ;
#6044 = CARTESIAN_POINT ( 'NONE',  ( -10.04416526290807710, -25.50457296725819489, 5.794927507916957765 ) ) ;
#6045 = DIRECTION ( 'NONE',  ( 0.000000000000000000, 0.7071067811865456854, 0.7071067811865494601 ) ) ;
#6046 = CARTESIAN_POINT ( 'NONE',  ( -1.040834085586084257E-14, -46.24364068711926024, -10.75835931288103886 ) ) ;
#6047 = CARTESIAN_POINT ( 'NONE',  ( -4.189131392896629613, 26.90500129688593134, 59.57932772728315030 ) ) ;
#6048 = DIRECTION ( 'NONE',  ( -1.000000000000000000, 0.000000000000000000, 0.000000000000000000 ) ) ;
#6049 = CARTESIAN_POINT ( 'NONE',  ( 1.461580736456473684, 65.46158073645646880, 46.25000000109246656 ) ) ;
#6050 = DIRECTION ( 'NONE',  ( -0.000000000000000000, 0.000000000000000000, 1.000000000000000000 ) ) ;
#6051 = CARTESIAN_POINT ( 'NONE',  ( 0.1249999999999895917, 33.84290755733280065, 52.64142146683631296 ) ) ;
#6052 = ORIENTED_EDGE ( 'NONE', *, *, #1617, .T. ) ;
#6053 = EDGE_LOOP ( 'NONE', ( #15714, #14119, #18993, #14136 ) ) ;
#6054 = CARTESIAN_POINT ( 'NONE',  ( -11.35725562635139418, -29.97976432393972601, 24.17382249208304046 ) ) ;
#6055 = EDGE_CURVE ( 'NONE', #13407, #9088, #3138, .T. ) ;
#6056 = CARTESIAN_POINT ( 'NONE',  ( -1.767766952966370209, 65.76776695296638309, 47.49999999999999289 ) ) ;
#6058 = ORIENTED_EDGE ( 'NONE', *, *, #17781, .T. ) ;
#6057 = ORIENTED_EDGE ( 'NONE', *, *, #3312, .F. ) ;
#6059 = CARTESIAN_POINT ( 'NONE',  ( -16.64274437364856496, -26.51566270880199738, 17.82617750791695954 ) ) ;
#6060 = DIRECTION ( 'NONE',  ( 1.000000000000000000, -0.000000000000000000, -0.000000000000000000 ) ) ;
#6061 = CARTESIAN_POINT ( 'NONE',  ( -22.04416526290807710, -25.71081734191525925, 39.48242750791695244 ) ) ;
#6062 = LINE ( 'NONE', #3317, #6344 ) ;
#6063 = CARTESIAN_POINT ( 'NONE',  ( -1.461580736456473462, 62.53841926354353120, 47.25000000109247367 ) ) ;
#6064 = ORIENTED_EDGE ( 'NONE', *, *, #8117, .T. ) ;
#6065 = EDGE_LOOP ( 'NONE', ( #15366, #2806, #17176, #4348, #10583, #77, #16992, #5867, #17595, #16976, #12350, #1961, #1935, #3020, #10520, #5796 ) ) ;
#6066 = EDGE_CURVE ( 'NONE', #15191, #10270, #15648, .T. ) ;
#6067 = CARTESIAN_POINT ( 'NONE',  ( -2.500000000000001776, 64.00000000000000000, 46.00000000000000000 ) ) ;
#6068 = FACE_OUTER_BOUND ( 'NONE', #16474, .T. ) ;
#6069 = ORIENTED_EDGE ( 'NONE', *, *, #2927, .T. ) ;
#6070 = DIRECTION ( 'NONE',  ( 0.000000000000000000, 0.000000000000000000, 1.000000000000000000 ) ) ;
#6071 = DIRECTION ( 'NONE',  ( 0.000000000000000000, 1.000000000000000000, 0.000000000000000000 ) ) ;
#6072 = CARTESIAN_POINT ( 'NONE',  ( -2.066987300000001415, 64.00000000000000000, 46.55000000109247082 ) ) ;
#6073 = APPLICATION_CONTEXT ( 'automotive_design' ) ;
#6074 = FACE_BOUND ( 'NONE', #9981, .T. ) ;
#6075 = DIRECTION ( 'NONE',  ( -1.047444401652940007E-14, -0.7071067811865495711, 0.7071067811865454633 ) ) ;
#6076 = EDGE_CURVE ( 'NONE', #14374, #4696, #7617, .T. ) ;
#6077 = ORIENTED_EDGE ( 'NONE', *, *, #12009, .T. ) ;
#6079 = ORIENTED_EDGE ( 'NONE', *, *, #6730, .T. ) ;
#6078 = ORIENTED_EDGE ( 'NONE', *, *, #4748, .F. ) ;
#6080 = CARTESIAN_POINT ( 'NONE',  ( -8.855408670957631401, -20.64274437364852943, 15.63867750791696132 ) ) ;
#6081 = DIRECTION ( 'NONE',  ( 0.000000000000000000, 0.000000000000000000, -1.000000000000000000 ) ) ;
#6082 = ORIENTED_EDGE ( 'NONE', *, *, #8871, .T. ) ;
#6083 = VERTEX_POINT ( 'NONE', #11318 ) ;
#6084 = CARTESIAN_POINT ( 'NONE',  ( -13.35725562635141195, -26.51566270880198672, 18.92382249208304401 ) ) ;
#6085 = CARTESIAN_POINT ( 'NONE',  ( -13.28918265808472299, -31.04416526290805933, 22.41992750791695954 ) ) ;
#6086 = CARTESIAN_POINT ( 'NONE',  ( -40.00000000000000711, 110.0000000000000000, 30.00000000000000000 ) ) ;
#6087 = CARTESIAN_POINT ( 'NONE',  ( 20.00000000000000355, -52.00000000000000711, 1.500000000000000000 ) ) ;
#6088 = EDGE_CURVE ( 'NONE', #1710, #12028, #655, .T. ) ;
#6089 = ORIENTED_EDGE ( 'NONE', *, *, #847, .T. ) ;
#6090 = CARTESIAN_POINT ( 'NONE',  ( -17.31681416490115311, -26.07549068051209318, 18.04492750791696309 ) ) ;
#6091 = LINE ( 'NONE', #4627, #5049 ) ;
#6092 = ORIENTED_EDGE ( 'NONE', *, *, #18557, .F. ) ;
#6093 = DIRECTION ( 'NONE',  ( -1.000000000000000000, 0.000000000000000000, -1.156482317317871725E-16 ) ) ;
#6094 = VERTEX_POINT ( 'NONE', #17126 ) ;
#6095 = CARTESIAN_POINT ( 'NONE',  ( -25.00000000000001421, 107.3545527679194436, 47.49999999999997868 ) ) ;
#6096 = FACE_OUTER_BOUND ( 'NONE', #11184, .T. ) ;
#6097 = CARTESIAN_POINT ( 'NONE',  ( -15.00000000000000000, 47.00000000000000711, 33.99999999999999289 ) ) ;
#6098 = CARTESIAN_POINT ( 'NONE',  ( 5.799999999999985612, 29.65425233947092920, 56.47747564417436195 ) ) ;
#6099 = LINE ( 'NONE', #10493, #8490 ) ;
#6100 =( GEOMETRIC_REPRESENTATION_CONTEXT ( 3 ) GLOBAL_UNCERTAINTY_ASSIGNED_CONTEXT ( ( #17466 ) ) GLOBAL_UNIT_ASSIGNED_CONTEXT ( ( #7519, #7319, #1245 ) ) REPRESENTATION_CONTEXT ( 'NONE', 'WORKASPACE' ) );
#6101 = CARTESIAN_POINT ( 'NONE',  ( -17.35725562635144215, -19.58745947852648683, 40.57617750791696665 ) ) ;
#6102 = VECTOR ( 'NONE', #2621, 1000.000000000000000 ) ;
#6103 = CARTESIAN_POINT ( 'NONE',  ( -15.16482700510263371, -18.99999999999997868, 42.98632249208304046 ) ) ;
#6104 = CARTESIAN_POINT ( 'NONE',  ( -17.35725562635144215, -19.58745947852648683, 14.32617750791695777 ) ) ;
#6105 = LINE ( 'NONE', #9033, #7721 ) ;
#6106 = ORIENTED_EDGE ( 'NONE', *, *, #7816, .F. ) ;
#6107 = PRODUCT_DEFINITION_CONTEXT ( 'detailed design', #2068, 'design' ) ;
#6108 = CARTESIAN_POINT ( 'NONE',  ( -14.83517299489735741, -28.99999999999998224, 24.61132249208304401 ) ) ;
#6109 = CARTESIAN_POINT ( 'NONE',  ( -0.8561741729129465073, 61.93301270000000613, 44.90000000109247225 ) ) ;
#6110 = CARTESIAN_POINT ( 'NONE',  ( -12.31951028609536536, -25.35725562635139596, 23.73632249208304401 ) ) ;
#6111 = AXIS2_PLACEMENT_3D ( 'NONE', #7793, #18088, #1913 ) ;
#6112 = DIRECTION ( 'NONE',  ( -1.000000000000000000, -0.000000000000000000, -0.000000000000000000 ) ) ;
#6113 = VERTEX_POINT ( 'NONE', #3874 ) ;
#6114 = AXIS2_PLACEMENT_3D ( 'NONE', #14044, #8081, #335 ) ;
#6115 = CARTESIAN_POINT ( 'NONE',  ( -13.80790879128036153, -18.12502140183178412, 9.743381756881012649E-15 ) ) ;
#6116 = VERTEX_POINT ( 'NONE', #9842 ) ;
#6117 = DIRECTION ( 'NONE',  ( 0.000000000000000000, -0.000000000000000000, 1.000000000000000000 ) ) ;
#6118 = FACE_OUTER_BOUND ( 'NONE', #3223, .T. ) ;
#6119 = DIRECTION ( 'NONE',  ( -1.000000000000000000, 2.470246229790980797E-15, -2.470246229790967386E-15 ) ) ;
#6120 = CARTESIAN_POINT ( 'NONE',  ( 1.461580736456473906, 62.53841926354353120, 47.65000000109247225 ) ) ;
#6121 = CARTESIAN_POINT ( 'NONE',  ( 2.500000000000002220, 62.96446609406726935, 47.14999999999999858 ) ) ;
#6122 = DIRECTION ( 'NONE',  ( 0.000000000000000000, -1.000000000000000000, 0.000000000000000000 ) ) ;
#6123 = VECTOR ( 'NONE', #8158, 1000.000000000000000 ) ;
#6124 = AXIS2_PLACEMENT_3D ( 'NONE', #12697, #15560, #10940 ) ;
#6125 = ORIENTED_EDGE ( 'NONE', *, *, #3628, .T. ) ;
#6126 = EDGE_CURVE ( 'NONE', #12927, #8090, #8384, .T. ) ;
#6127 = EDGE_CURVE ( 'NONE', #17145, #3695, #13755, .T. ) ;
#6128 =( BOUNDED_CURVE ( )  B_SPLINE_CURVE ( 2, ( #3802, #9944, #11227, #12897, #15943, #12986, #14369, #6927, #7018 ),
 .UNSPECIFIED., .F., .F. ) 
 B_SPLINE_CURVE_WITH_KNOTS ( ( 3, 2, 2, 2, 3 ),
 ( 0.000000000000000000, 0.01785714285714289085, 0.03571428571428578169, 0.05357142857142867254, 0.07142857142857156338 ),
 .UNSPECIFIED. ) 
 CURVE ( )  GEOMETRIC_REPRESENTATION_ITEM ( )  RATIONAL_B_SPLINE_CURVE ( ( 1.000000000000000000, 0.9238795325112867385, 1.000000000000000000, 0.9238795325112867385, 1.000000000000000000, 0.9238795325112867385, 1.000000000000000000, 0.9238795325112861834, 1.000000000000000666 ) ) 
 REPRESENTATION_ITEM ( '' )  );
#6129 = DIRECTION ( 'NONE',  ( 0.000000000000000000, 0.000000000000000000, 1.000000000000000000 ) ) ;
#6130 = CARTESIAN_POINT ( 'NONE',  ( -17.64274437364855430, -28.24771351637087236, 23.07617750791695954 ) ) ;
#6131 = CARTESIAN_POINT ( 'NONE',  ( -11.21908421996108629, -20.46040770435011069, 15.41992750791695954 ) ) ;
#6132 = CARTESIAN_POINT ( 'NONE',  ( -2.500000000000000888, 62.96446609406726935, 48.55000000218494449 ) ) ;
#6133 = EDGE_CURVE ( 'NONE', #578, #9541, #4705, .T. ) ;
#6134 = CARTESIAN_POINT ( 'NONE',  ( -10.75228648362912232, -21.35725562635138530, 7.111322492083040459 ) ) ;
#6135 = CARTESIAN_POINT ( 'NONE',  ( -1.461580736456473462, 62.53841926354353120, 45.85000000109246798 ) ) ;
#6136 = CARTESIAN_POINT ( 'NONE',  ( -9.999999999999994671, -24.16482700510257686, 0.3261775079169582647 ) ) ;
#6137 = ADVANCED_FACE ( 'NONE', ( #11600 ), #6034, .T. ) ;
#6138 = PLANE ( 'NONE',  #7019 ) ;
#6139 = VECTOR ( 'NONE', #18132, 1000.000000000000000 ) ;
#6140 = CARTESIAN_POINT ( 'NONE',  ( -14.83517299489739649, -18.99999999999997868, 20.01367750791695954 ) ) ;
#6141 = LINE ( 'NONE', #7608, #8726 ) ;
#6142 = DIRECTION ( 'NONE',  ( 0.000000000000000000, 1.000000000000000000, 0.000000000000000000 ) ) ;
#6143 = AXIS2_PLACEMENT_3D ( 'NONE', #12388, #141, #7690 ) ;
#6144 = CARTESIAN_POINT ( 'NONE',  ( 2.066987300000001859, 64.85617417291294373, 47.80000000109247082 ) ) ;
#6145 = DIRECTION ( 'NONE',  ( 1.000000000000000000, -0.000000000000000000, -0.000000000000000000 ) ) ;
#6146 = DIRECTION ( 'NONE',  ( -1.000000000000000000, 0.000000000000000000, 0.000000000000000000 ) ) ;
#6147 = CARTESIAN_POINT ( 'NONE',  ( 3.796994071234847710E-16, 61.93301269999999903, 45.15000000109247225 ) ) ;
#6148 = CARTESIAN_POINT ( 'NONE',  ( -1.265664690411616068E-16, 66.06698730000000808, 49.55000000109247082 ) ) ;
#6149 = EDGE_CURVE ( 'NONE', #12140, #17031, #11697, .T. ) ;
#6150 = DIRECTION ( 'NONE',  ( -7.304098846218135653E-17, 0.000000000000000000, 1.000000000000000000 ) ) ;
#6151 = LINE ( 'NONE', #8089, #10826 ) ;
#6152 = ORIENTED_EDGE ( 'NONE', *, *, #6863, .F. ) ;
#6153 = ORIENTED_EDGE ( 'NONE', *, *, #7072, .F. ) ;
#6154 = CARTESIAN_POINT ( 'NONE',  ( -17.04047135212050890, -17.04416526290807710, 11.26757249208304046 ) ) ;
#6155 =( NAMED_UNIT ( * ) PLANE_ANGLE_UNIT ( ) SI_UNIT ( $, .RADIAN. ) );
#6156 = CARTESIAN_POINT ( 'NONE',  ( -16.50457296725825174, -19.04416526290807354, 11.26757249208304046 ) ) ;
#6158 = ORIENTED_EDGE ( 'NONE', *, *, #7349, .T. ) ;
#6157 = ORIENTED_EDGE ( 'NONE', *, *, #5325, .F. ) ;
#6159 = PRODUCT_DEFINITION_SHAPE ( 'NONE', 'NONE',  #7639 ) ;
#6160 = ADVANCED_FACE ( 'NONE', ( #16215 ), #17016, .T. ) ;
#6161 = CARTESIAN_POINT ( 'NONE',  ( -17.95583473709191580, -23.03132541760400898, 13.66992750791696309 ) ) ;
#6162 = CARTESIAN_POINT ( 'NONE',  ( -1.265664690411616068E-16, 66.06698730000000808, 44.75000000109247367 ) ) ;
#6163 = CARTESIAN_POINT ( 'NONE',  ( -7.955834737091903364, -25.71081734191518464, 7.767572492083039570 ) ) ;
#6164 = CARTESIAN_POINT ( 'NONE',  ( -1.461580736456473906, 65.46158073645646880, 49.45000000109246940 ) ) ;
#6165 = CARTESIAN_POINT ( 'NONE',  ( -1.265664690411616068E-16, 66.06698730000000808, 47.75000000109246656 ) ) ;
#6166 = ORIENTED_EDGE ( 'NONE', *, *, #15643, .T. ) ;
#6167 = VERTEX_POINT ( 'NONE', #3069 ) ;
#6168 = CARTESIAN_POINT ( 'NONE',  ( -40.00000000000000711, 110.0000000000000000, 13.50000000000000178 ) ) ;
#6169 = ORIENTED_EDGE ( 'NONE', *, *, #13265, .T. ) ;
#6170 = VERTEX_POINT ( 'NONE', #5916 ) ;
#6171 = LINE ( 'NONE', #8999, #4997 ) ;
#6172 = CARTESIAN_POINT ( 'NONE',  ( -50.00000000000001421, 17.99999999999993250, 59.99999999999997868 ) ) ;
#6173 = VECTOR ( 'NONE', #10474, 1000.000000000000000 ) ;
#6174 = CARTESIAN_POINT ( 'NONE',  ( 2.066987300000001415, 64.00000000000000000, 46.15000000109247225 ) ) ;
#6175 = EDGE_CURVE ( 'NONE', #1607, #3132, #12795, .T. ) ;
#6176 = AXIS2_PLACEMENT_3D ( 'NONE', #5443, #7098, #15924 ) ;
#6177 = EDGE_CURVE ( 'NONE', #6482, #8924, #16108, .T. ) ;
#6178 = DIRECTION ( 'NONE',  ( 0.000000000000000000, 0.000000000000000000, 1.000000000000000000 ) ) ;
#6179 = ADVANCED_FACE ( 'NONE', ( #2770 ), #7287, .F. ) ;
#6180 = CARTESIAN_POINT ( 'NONE',  ( 37.49999999999999289, 107.3545527679194436, 24.99999999999998579 ) ) ;
#6181 = ORIENTED_EDGE ( 'NONE', *, *, #1761, .F. ) ;
#6183 = ORIENTED_EDGE ( 'NONE', *, *, #17872, .F. ) ;
#6182 = EDGE_LOOP ( 'NONE', ( #15085, #6152, #8159, #5895 ) ) ;
#6184 = EDGE_CURVE ( 'NONE', #8734, #2520, #17776, .T. ) ;
#6185 = CARTESIAN_POINT ( 'NONE',  ( -12.95952864787955150, -17.04416526290805933, 9.732427507916955989 ) ) ;
#6186 =( NAMED_UNIT ( * ) PLANE_ANGLE_UNIT ( ) SI_UNIT ( $, .RADIAN. ) );
#6187 = ORIENTED_EDGE ( 'NONE', *, *, #14376, .T. ) ;
#6188 = EDGE_LOOP ( 'NONE', ( #553, #2025 ) ) ;
#6189 = CARTESIAN_POINT ( 'NONE',  ( -12.68318583509882380, -26.07549068051207541, 13.45507249208304401 ) ) ;
#6190 =( GEOMETRIC_REPRESENTATION_CONTEXT ( 3 ) GLOBAL_UNCERTAINTY_ASSIGNED_CONTEXT ( ( #7693 ) ) GLOBAL_UNIT_ASSIGNED_CONTEXT ( ( #8983, #11717, #14970 ) ) REPRESENTATION_CONTEXT ( 'NONE', 'WORKASPACE' ) );
#6191 = CARTESIAN_POINT ( 'NONE',  ( -1.461580736456473906, 65.46158073645646880, 47.85000000109246798 ) ) ;
#6192 = CARTESIAN_POINT ( 'NONE',  ( -41.00000000000000000, 0.000000000000000000, -67.72004514666936359 ) ) ;
#6193 = VERTEX_POINT ( 'NONE', #14939 ) ;
#6194 = CARTESIAN_POINT ( 'NONE',  ( -12.68318583509884157, -21.92450931948787485, 20.66992750791696665 ) ) ;
#6195 = DIRECTION ( 'NONE',  ( 1.000000000000000000, 0.000000000000000000, 0.000000000000000000 ) ) ;
#6196 = ORIENTED_EDGE ( 'NONE', *, *, #4140, .F. ) ;
#6197 = CARTESIAN_POINT ( 'NONE',  ( 2.500000000000002220, 62.96446609406726225, 45.54999999999999005 ) ) ;
#6198 = EDGE_LOOP ( 'NONE', ( #12639, #14500, #12662, #7559 ) ) ;
#6199 = EDGE_CURVE ( 'NONE', #19316, #16247, #11784, .T. ) ;
#6200 = CARTESIAN_POINT ( 'NONE',  ( -40.00000000000000000, 53.00000000000000711, -50.00000000000000000 ) ) ;
#6201 = LINE ( 'NONE', #7361, #486 ) ;
#6202 = DIRECTION ( 'NONE',  ( -1.541976423090495880E-16, 0.000000000000000000, 1.000000000000000000 ) ) ;
#6203 = ITEM_DEFINED_TRANSFORMATION ( 'NONE', 'NONE', #7994,  #1791 ) ;
#6204 = DIRECTION ( 'NONE',  ( 0.000000000000000000, 0.000000000000000000, 1.000000000000000000 ) ) ;
#6205 = CARTESIAN_POINT ( 'NONE',  ( -11.21908421996108629, -20.46040770435011069, 36.41992750791695954 ) ) ;
#6206 = DIRECTION ( 'NONE',  ( -0.000000000000000000, 1.000000000000000000, -0.000000000000000000 ) ) ;
#6207 = CARTESIAN_POINT ( 'NONE',  ( -11.46040770435012668, -27.78091578003887463, 21.98242750791695244 ) ) ;
#6208 = FACE_OUTER_BOUND ( 'NONE', #12180, .T. ) ;
#6209 = ORIENTED_EDGE ( 'NONE', *, *, #17847, .F. ) ;
#6210 = CARTESIAN_POINT ( 'NONE',  ( -10.75228648362912232, -21.35725562635138530, 17.61132249208304401 ) ) ;
#6211 = CARTESIAN_POINT ( 'NONE',  ( -1.530808498934192803E-16, 66.50000000000000000, 47.39999999999999858 ) ) ;
#6212 = CARTESIAN_POINT ( 'NONE',  ( -17.51566270880199738, -25.64274437364856496, 25.48632249208304401 ) ) ;
#6213 = LINE ( 'NONE', #1507, #4077 ) ;
#6214 = ORIENTED_EDGE ( 'NONE', *, *, #3470, .T. ) ;
#6215 = LINE ( 'NONE', #19347, #9680 ) ;
#6216 = VERTEX_POINT ( 'NONE', #4352 ) ;
#6217 = ADVANCED_FACE ( 'NONE', ( #16403 ), #9048, .T. ) ;
#6218 = CARTESIAN_POINT ( 'NONE',  ( -7.999999999999996447, -32.00000000000000711, 1.500000000000000000 ) ) ;
#6219 = DIRECTION ( 'NONE',  ( -1.000000000000000000, 0.000000000000000000, -0.000000000000000000 ) ) ;
#6220 = DIRECTION ( 'NONE',  ( 0.000000000000000000, 0.000000000000000000, -1.000000000000000000 ) ) ;
#6221 = CARTESIAN_POINT ( 'NONE',  ( 1.461580736456473906, 62.53841926354353120, 45.25000000109247367 ) ) ;
#6222 = SURFACE_STYLE_USAGE ( .BOTH. , #12387 ) ;
#6223 = DIRECTION ( 'NONE',  ( 0.000000000000000000, -1.000000000000000000, 0.000000000000000000 ) ) ;
#6224 = FACE_OUTER_BOUND ( 'NONE', #18804, .T. ) ;
#6225 = EDGE_LOOP ( 'NONE', ( #13723, #3360, #8887, #2920, #5951, #17856 ) ) ;
#6226 = VECTOR ( 'NONE', #8102, 1000.000000000000000 ) ;
#6227 = CARTESIAN_POINT ( 'NONE',  ( 0.000000000000000000, 0.000000000000000000, 0.000000000000000000 ) ) ;
#6228 = CARTESIAN_POINT ( 'NONE',  ( -11.46040770435012668, -27.78091578003887463, 21.98242750791695244 ) ) ;
#6229 = CARTESIAN_POINT ( 'NONE',  ( -1.530808498934192803E-16, 66.50000000000000000, 44.30000000218494449 ) ) ;
#6230 = CARTESIAN_POINT ( 'NONE',  ( -17.64274437364858983, -19.75228648362910633, 21.54882249208304401 ) ) ;
#6231 = CARTESIAN_POINT ( 'NONE',  ( -1.461580736456473462, 62.53841926354353120, 46.65000000109247225 ) ) ;
#6232 = CARTESIAN_POINT ( 'NONE',  ( -19.24771351637089367, -21.35725562635142438, 13.88867750791695954 ) ) ;
#6233 = DIRECTION ( 'NONE',  ( 0.000000000000000000, 0.000000000000000000, 1.000000000000000000 ) ) ;
#6235 = CARTESIAN_POINT ( 'NONE',  ( -9.999999999999994671, -24.16482700510257686, 16.07617750791695954 ) ) ;
#6234 = VECTOR ( 'NONE', #2899, 1000.000000000000114 ) ;
#6236 = CYLINDRICAL_SURFACE ( 'NONE', #9667, 1.599999999999997202 ) ;
#6237 = FACE_OUTER_BOUND ( 'NONE', #5377, .T. ) ;
#6238 = CARTESIAN_POINT ( 'NONE',  ( -1.461580736456473906, 65.46158073645646880, 47.25000000109246656 ) ) ;
#6239 = LINE ( 'NONE', #2900, #8396 ) ;
#6240 = VECTOR ( 'NONE', #11911, 1000.000000000000000 ) ;
#6241 = CARTESIAN_POINT ( 'NONE',  ( -41.00000000000000711, 110.0000000000000000, -11.50000000000000000 ) ) ;
#6242 = PLANE ( 'NONE',  #9602 ) ;
#6243 = CARTESIAN_POINT ( 'NONE',  ( 2.066987300000001859, 64.85617417291294373, 48.60000000109246798 ) ) ;
#6244 = DIRECTION ( 'NONE',  ( 1.000000000000000000, -0.000000000000000000, -0.000000000000000000 ) ) ;
#6245 = ORIENTED_EDGE ( 'NONE', *, *, #12226, .T. ) ;
#6246 = ORIENTED_EDGE ( 'NONE', *, *, #8922, .F. ) ;
#6247 = CARTESIAN_POINT ( 'NONE',  ( -7.999999999999996447, -23.83517299489733432, 12.79882249208303691 ) ) ;
#6248 = ADVANCED_FACE ( 'NONE', ( #1408 ), #19155, .T. ) ;
#6249 = VECTOR ( 'NONE', #7384, 1000.000000000000000 ) ;
#6250 = CARTESIAN_POINT ( 'NONE',  ( -19.95583473709190514, -25.50457296725823042, 4.705072492083040459 ) ) ;
#6251 = EDGE_LOOP ( 'NONE', ( #9186, #1440, #16360, #2422 ) ) ;
#6252 = CARTESIAN_POINT ( 'NONE',  ( -13.35725562635142794, -21.48433729119796709, 15.20117750791696132 ) ) ;
#6253 = CARTESIAN_POINT ( 'NONE',  ( -2.492551403682614186, 27.92836399182264273, 58.20336399182264131 ) ) ;
#6254 = CARTESIAN_POINT ( 'NONE',  ( -11.35725562635139418, -29.97976432393972601, 18.92382249208303691 ) ) ;
#6255 = VECTOR ( 'NONE', #3656, 1000.000000000000000 ) ;
#6256 = AXIS2_PLACEMENT_3D ( 'NONE', #14593, #8807, #2438 ) ;
#6257 = CARTESIAN_POINT ( 'NONE',  ( 2.500000000000001776, 64.00000000000000000, 47.99999999999999289 ) ) ;
#6258 = CARTESIAN_POINT ( 'NONE',  ( -2.066987300000001415, 64.00000000000000000, 45.55000000109246372 ) ) ;
#6259 = ORIENTED_EDGE ( 'NONE', *, *, #10599, .T. ) ;
#6260 = VERTEX_POINT ( 'NONE', #2968 ) ;
#6261 = CYLINDRICAL_SURFACE ( 'NONE', #932, 2.999999999999999112 ) ;
#6262 = DIRECTION ( 'NONE',  ( 0.000000000000000000, -1.000000000000000000, 0.000000000000000000 ) ) ;
#6263 = ORIENTED_EDGE ( 'NONE', *, *, #18213, .T. ) ;
#6264 = CARTESIAN_POINT ( 'NONE',  ( 2.066987300000001415, 64.00000000000000000, 49.15000000109247225 ) ) ;
#6265 = CARTESIAN_POINT ( 'NONE',  ( 14.33926609531033058, -43.78611686177728046, 1.500000000000000000 ) ) ;
#6266 = ADVANCED_FACE ( 'NONE', ( #12081 ), #6023, .F. ) ;
#6267 = FACE_OUTER_BOUND ( 'NONE', #3647, .T. ) ;
#6268 = DIRECTION ( 'NONE',  ( 1.000000000000000000, -0.000000000000000000, -0.000000000000000000 ) ) ;
#6269 = AXIS2_PLACEMENT_3D ( 'NONE', #1487, #13232, #13425 ) ;
#6270 = CARTESIAN_POINT ( 'NONE',  ( -37.50000000000002132, 107.3545527679194436, -25.00000000000002132 ) ) ;
#6271 = ORIENTED_EDGE ( 'NONE', *, *, #16937, .T. ) ;
#6273 = ORIENTED_EDGE ( 'NONE', *, *, #18853, .F. ) ;
#6272 = EDGE_LOOP ( 'NONE', ( #7222, #15779, #5883, #15459 ) ) ;
#6274 = CARTESIAN_POINT ( 'NONE',  ( -16.71081734191527346, -16.95583473709190159, 19.79492750791695954 ) ) ;
#6275 = ORIENTED_EDGE ( 'NONE', *, *, #2439, .F. ) ;
#6277 = ORIENTED_EDGE ( 'NONE', *, *, #1714, .T. ) ;
#6276 = ORIENTED_EDGE ( 'NONE', *, *, #17526, .F. ) ;
#6278 = CARTESIAN_POINT ( 'NONE',  ( -17.68048971390462754, -22.64274437364856496, 15.86132249208304401 ) ) ;
#6279 = CARTESIAN_POINT ( 'NONE',  ( -14.83517299489740715, -16.99999999999997868, 9.513677507916955989 ) ) ;
#6280 = ADVANCED_FACE ( 'NONE', ( #8946 ), #4551, .F. ) ;
#6281 = ADVANCED_FACE ( 'NONE', ( #7585 ), #16203, .F. ) ;
#6282 = CARTESIAN_POINT ( 'NONE',  ( 1.461580736456473906, 62.53841926354353120, 48.25000000109246656 ) ) ;
#6283 = CARTESIAN_POINT ( 'NONE',  ( -12.50000000000000000, -35.50000000000000000, 5.500000000000000000 ) ) ;
#6284 = ORIENTED_EDGE ( 'NONE', *, *, #10219, .F. ) ;
#6285 = EDGE_CURVE ( 'NONE', #11383, #7718, #7888, .T. ) ;
#6286 = CARTESIAN_POINT ( 'NONE',  ( -13.64274437364856141, -26.68048971390460622, 16.95117750791696309 ) ) ;
#6287 = VECTOR ( 'NONE', #16164, 1000.000000000000000 ) ;
#6288 =( NAMED_UNIT ( * ) PLANE_ANGLE_UNIT ( ) SI_UNIT ( $, .RADIAN. ) );
#6289 = EDGE_LOOP ( 'NONE', ( #16238, #19392, #5277, #128, #14016 ) ) ;
#6290 = CARTESIAN_POINT ( 'NONE',  ( 1.767766952966370653, 62.23223304703363112, 45.50000000000000000 ) ) ;
#6291 = ORIENTED_EDGE ( 'NONE', *, *, #7103, .F. ) ;
#6292 = CARTESIAN_POINT ( 'NONE',  ( 7.500000000000005329, -26.00000000000000000, 4.500000000000000888 ) ) ;
#6293 = CARTESIAN_POINT ( 'NONE',  ( 1.035533905932738197, 66.50000000000000000, 46.54999999999999716 ) ) ;
#6294 = DIRECTION ( 'NONE',  ( -1.000000000000000000, -0.000000000000000000, -0.000000000000000000 ) ) ;
#6295 = CARTESIAN_POINT ( 'NONE',  ( -24.00000000000000000, 53.00000000000000711, 30.00000000000000000 ) ) ;
#6296 = CARTESIAN_POINT ( 'NONE',  ( -2.066987300000001415, 64.00000000000000000, 47.15000000109247225 ) ) ;
#6297 = CONTEXT_DEPENDENT_SHAPE_REPRESENTATION ( #16723, #7558 ) ;
#6298 = DIRECTION ( 'NONE',  ( 5.782411586589357392E-17, -0.000000000000000000, 1.000000000000000000 ) ) ;
#6299 = CARTESIAN_POINT ( 'NONE',  ( -25.00000000000000000, 110.0000000000000000, 30.00000000000000000 ) ) ;
#6300 = VECTOR ( 'NONE', #5439, 1000.000000000000000 ) ;
#6301 = CARTESIAN_POINT ( 'NONE',  ( -17.64274437364855430, -28.24771351637087236, 38.82617750791695954 ) ) ;
#6302 = CARTESIAN_POINT ( 'NONE',  ( -1.040834085586084257E-14, 25.49999999999998934, 52.50000000000000000 ) ) ;
#6303 = ORIENTED_EDGE ( 'NONE', *, *, #17489, .F. ) ;
#6304 = CARTESIAN_POINT ( 'NONE',  ( -17.64274437364855430, -28.24771351637087236, 12.57617750791695777 ) ) ;
#6305 = VECTOR ( 'NONE', #12433, 1000.000000000000000 ) ;
#6306 = CARTESIAN_POINT ( 'NONE',  ( -50.00000000000002132, 30.87867965644036516, 42.87867965644034030 ) ) ;
#6307 = ORIENTED_EDGE ( 'NONE', *, *, #10956, .F. ) ;
#6308 = CARTESIAN_POINT ( 'NONE',  ( -17.64274437364858983, -19.75228648362910633, 11.04882249208304046 ) ) ;
#6309 = EDGE_CURVE ( 'NONE', #9861, #9708, #1700, .T. ) ;
#6310 = AXIS2_PLACEMENT_3D ( 'NONE', #4226, #2847, #17855 ) ;
#6311 = CARTESIAN_POINT ( 'NONE',  ( -18.04416526290808775, -23.36097942780924441, 20.89257249208304046 ) ) ;
#6312 = DIRECTION ( 'NONE',  ( 1.000000000000000000, 0.000000000000000000, 0.000000000000000000 ) ) ;
#6313 = ORIENTED_EDGE ( 'NONE', *, *, #6867, .T. ) ;
#6314 = VECTOR ( 'NONE', #4143, 1000.000000000000000 ) ;
#6315 = FACE_OUTER_BOUND ( 'NONE', #5778, .T. ) ;
#6316 = ORIENTED_EDGE ( 'NONE', *, *, #18246, .F. ) ;
#6317 = DIRECTION ( 'NONE',  ( 0.000000000000000000, 0.000000000000000000, 1.000000000000000000 ) ) ;
#6318 = CARTESIAN_POINT ( 'NONE',  ( -4.000000000000001776, 67.00000000000000000, 30.00000000000000000 ) ) ;
#6319 = PRESENTATION_LAYER_ASSIGNMENT (  '', '', ( #15086 ) ) ;
#6320 = PLANE ( 'NONE',  #8178 ) ;
#6321 = LINE ( 'NONE', #1805, #8157 ) ;
#6322 = VECTOR ( 'NONE', #15847, 1000.000000000000000 ) ;
#6323 = CARTESIAN_POINT ( 'NONE',  ( -50.00000000000002132, 30.00000000000000355, 59.99999999999997868 ) ) ;
#6324 = CARTESIAN_POINT ( 'NONE',  ( -0.9999999999999945599, -36.00000000000000711, 4.500000000000000888 ) ) ;
#6325 = CARTESIAN_POINT ( 'NONE',  ( -24.00000000000000000, 53.00000000000000711, -38.50000000000000711 ) ) ;
#6326 = CIRCLE ( 'NONE', #7897, 1.249999999999999334 ) ;
#6327 = ADVANCED_FACE ( 'NONE', ( #9149 ), #11002, .T. ) ;
#6328 = UNCERTAINTY_MEASURE_WITH_UNIT (LENGTH_MEASURE( 1.000000000000000082E-05 ), #18306, 'distance_accuracy_value', 'NONE');
#6329 = EDGE_LOOP ( 'NONE', ( #5416, #8401, #15992, #11647, #12021, #4585, #6020, #15429, #9022, #333, #1546, #10261, #792, #3128, #7036, #10853 ) ) ;
#6330 = AXIS2_PLACEMENT_3D ( 'NONE', #10151, #19097, #15866 ) ;
#6331 = DIRECTION ( 'NONE',  ( 6.123233995736766036E-17, -1.000000000000000000, 0.000000000000000000 ) ) ;
#6332 = CARTESIAN_POINT ( 'NONE',  ( -16.50457296725820555, -28.95583473709189448, 17.60742750791695599 ) ) ;
#6333 = CARTESIAN_POINT ( 'NONE',  ( 1.035533905932739751, 61.50000000000000000, 44.75000000218494023 ) ) ;
#6334 = CARTESIAN_POINT ( 'NONE',  ( -19.99999999999999645, -24.16482700510261949, 15.42382249208304046 ) ) ;
#6335 = CARTESIAN_POINT ( 'NONE',  ( -41.00000000000000711, 53.00000000000000711, 27.50000000000000000 ) ) ;
#6336 = EDGE_CURVE ( 'NONE', #13749, #9185, #1801, .T. ) ;
#6337 = CARTESIAN_POINT ( 'NONE',  ( -18.78091578003889950, -27.53959229564985378, 23.29492750791695954 ) ) ;
#6338 = LINE ( 'NONE', #3086, #16597 ) ;
#6339 = CARTESIAN_POINT ( 'NONE',  ( -19.95583473709191225, -22.49542703274176603, 13.66992750791695599 ) ) ;
#6340 = CARTESIAN_POINT ( 'NONE',  ( -11.25000000000000178, -35.50000000000000000, 5.000000000000003553 ) ) ;
#6341 = CYLINDRICAL_SURFACE ( 'NONE', #7899, 2.500000000000001776 ) ;
#6342 = CARTESIAN_POINT ( 'NONE',  ( -2.066987300000001415, 64.00000000000000000, 48.15000000109247225 ) ) ;
#6343 = LINE ( 'NONE', #17026, #15614 ) ;
#6344 = VECTOR ( 'NONE', #179, 1000.000000000000000 ) ;
#6345 = DIRECTION ( 'NONE',  ( 0.000000000000000000, -1.000000000000000000, 0.000000000000000000 ) ) ;
#6346 = CARTESIAN_POINT ( 'NONE',  ( 1.035533905932738197, 66.50000000000000000, 48.25000000218494733 ) ) ;
#6347 = CARTESIAN_POINT ( 'NONE',  ( 0.8561741729129460632, 66.06698729999999387, 46.30000000109247082 ) ) ;
#6348 = CARTESIAN_POINT ( 'NONE',  ( 12.99999999999999822, 0.000000000000000000, 0.000000000000000000 ) ) ;
#6349 = CLOSED_SHELL ( 'NONE', ( #17179, #14773, #17898, #14461, #9964, #10792, #11208, #6407, #6179, #302, #8220, #13820, #9503, #781, #1502, #2397, #18291 ) ) ;
#6351 = EDGE_LOOP ( 'NONE', ( #6696, #10283, #12733, #7946 ) ) ;
#6350 = ADVANCED_FACE ( 'NONE', ( #10711 ), #6413, .T. ) ;
#6352 = ORIENTED_EDGE ( 'NONE', *, *, #4130, .T. ) ;
#6353 = CARTESIAN_POINT ( 'NONE',  ( -21.14459132904239169, -20.64274437364858628, 26.36132249208303691 ) ) ;
#6354 = FILL_AREA_STYLE_COLOUR ( '', #16103 ) ;
#6355 = CARTESIAN_POINT ( 'NONE',  ( -13.82508104294702100, -18.95583473709188382, 6.455072492083042235 ) ) ;
#6356 = ORIENTED_EDGE ( 'NONE', *, *, #12943, .F. ) ;
#6357 = CARTESIAN_POINT ( 'NONE',  ( -15.16482700510260706, -26.99999999999998579, 22.63867750791696309 ) ) ;
#6358 = PLANE ( 'NONE',  #6124 ) ;
#6359 = CARTESIAN_POINT ( 'NONE',  ( -22.04416526290809486, -22.28918265808477628, 15.64257249208304223 ) ) ;
#6360 = CARTESIAN_POINT ( 'NONE',  ( 0.8561741729129460632, 66.06698729999999387, 49.30000000109246372 ) ) ;
#6361 = CARTESIAN_POINT ( 'NONE',  ( -2.066987300000001415, 63.14382582708705627, 46.40000000109246514 ) ) ;
#6362 = ORIENTED_EDGE ( 'NONE', *, *, #9870, .T. ) ;
#6363 = ORIENTED_EDGE ( 'NONE', *, *, #10106, .T. ) ;
#6364 = FACE_OUTER_BOUND ( 'NONE', #4387, .T. ) ;
#6365 = DIRECTION ( 'NONE',  ( 0.000000000000000000, -0.000000000000000000, -1.000000000000000000 ) ) ;
#6366 = ORIENTED_EDGE ( 'NONE', *, *, #3650, .T. ) ;
#6367 = PLANE ( 'NONE',  #8127 ) ;
#6368 = CARTESIAN_POINT ( 'NONE',  ( -25.00000000000000000, 110.0000000000000000, 14.50000000000000000 ) ) ;
#6369 = CARTESIAN_POINT ( 'NONE',  ( -7.999999999999986677, 68.00000000000000000, 45.00000000000000000 ) ) ;
#6370 = CARTESIAN_POINT ( 'NONE',  ( -0.9999999999999945599, -32.00000000000000000, 9.500000000000001776 ) ) ;
#6371 = CARTESIAN_POINT ( 'NONE',  ( -14.99999999999999645, 73.00000000000001421, 26.99999999999997868 ) ) ;
#6372 = EDGE_LOOP ( 'NONE', ( #6758, #3739, #17530, #12715 ) ) ;
#6374 = VERTEX_POINT ( 'NONE', #18379 ) ;
#6373 = ORIENTED_EDGE ( 'NONE', *, *, #9822, .T. ) ;
#6375 = CARTESIAN_POINT ( 'NONE',  ( -11.35725562635144925, -18.02023567606020293, 30.95117750791695954 ) ) ;
#6376 = VERTEX_POINT ( 'NONE', #6610 ) ;
#6377 = ORIENTED_EDGE ( 'NONE', *, *, #2203, .T. ) ;
#6378 = CARTESIAN_POINT ( 'NONE',  ( -14.36097942780925685, -20.95583473709189093, 16.95507249208304046 ) ) ;
#6379 = ADVANCED_FACE ( 'NONE', ( #10607 ), #9531, .F. ) ;
#6380 = EDGE_CURVE ( 'NONE', #9572, #6563, #334, .T. ) ;
#6381 = CARTESIAN_POINT ( 'NONE',  ( -7.955834737091916686, -22.28918265808470522, 10.60742750791695599 ) ) ;
#6382 = CARTESIAN_POINT ( 'NONE',  ( -1.461580736456473462, 62.53841926354353120, 47.25000000109247367 ) ) ;
#6383 = CARTESIAN_POINT ( 'NONE',  ( 14.99999999999998579, 73.00000000000001421, 23.99999999999997158 ) ) ;
#6384 = ORIENTED_EDGE ( 'NONE', *, *, #8459, .T. ) ;
#6385 = CARTESIAN_POINT ( 'NONE',  ( -17.07549068051210739, -21.68318583509881847, 19.35742750791695954 ) ) ;
#6386 = EDGE_CURVE ( 'NONE', #17001, #17276, #429, .T. ) ;
#6387 = ORIENTED_EDGE ( 'NONE', *, *, #7861, .T. ) ;
#6388 = CARTESIAN_POINT ( 'NONE',  ( -2.500000000000001776, 64.00000000000000000, 45.19999999999999574 ) ) ;
#6389 = VERTEX_POINT ( 'NONE', #3272 ) ;
#6390 = DIRECTION ( 'NONE',  ( 0.7071067811865495711, 8.659560562354957510E-17, -0.7071067811865455743 ) ) ;
#6391 = PLANE ( 'NONE',  #2509 ) ;
#6392 = DIRECTION ( 'NONE',  ( 0.000000000000000000, 0.000000000000000000, -1.000000000000000000 ) ) ;
#6393 = DIRECTION ( 'NONE',  ( 0.000000000000000000, 0.000000000000000000, 1.000000000000000000 ) ) ;
#6394 = DIRECTION ( 'NONE',  ( 0.000000000000000000, -1.000000000000000000, -0.000000000000000000 ) ) ;
#6395 = CARTESIAN_POINT ( 'NONE',  ( -2.066987300000001859, 64.85617417291294373, 47.90000000109247225 ) ) ;
#6396 = CARTESIAN_POINT ( 'NONE',  ( 24.99999999999999289, 0.000000000000000000, -42.50000000000001421 ) ) ;
#6397 = DIRECTION ( 'NONE',  ( 0.000000000000000000, 1.000000000000000000, 0.000000000000000000 ) ) ;
#6398 = CARTESIAN_POINT ( 'NONE',  ( -4.042620306204046443, 32.68389060951044911, 53.80012125920694643 ) ) ;
#6399 = EDGE_CURVE ( 'NONE', #14571, #10804, #233, .T. ) ;
#6400 = CARTESIAN_POINT ( 'NONE',  ( 1.890020143386967000, 65.62319932110614218, 45.00000000000000711 ) ) ;
#6401 = VERTEX_POINT ( 'NONE', #6218 ) ;
#6402 = EDGE_CURVE ( 'NONE', #11751, #9977, #12181, .T. ) ;
#6403 = CARTESIAN_POINT ( 'NONE',  ( -10.04416526290807710, -25.50457296725819489, 11.04492750791695421 ) ) ;
#6404 = LINE ( 'NONE', #9521, #6783 ) ;
#6405 = VERTEX_POINT ( 'NONE', #14043 ) ;
#6406 = CARTESIAN_POINT ( 'NONE',  ( -11.46040770435014977, -20.21908421996103655, 17.39257249208304401 ) ) ;
#6407 = ADVANCED_FACE ( 'NONE', ( #13950 ), #9334, .T. ) ;
#6408 = CARTESIAN_POINT ( 'NONE',  ( -17.95583473709190869, -24.96867458239598037, 20.45507249208304401 ) ) ;
#6409 = CARTESIAN_POINT ( 'NONE',  ( 34.99999999999999289, -6.000000000000000000, 47.49999999999997868 ) ) ;
#6410 = EDGE_LOOP ( 'NONE', ( #3333, #8231, #9292, #954 ) ) ;
#6411 = CARTESIAN_POINT ( 'NONE',  ( -41.00000000000000711, 53.00000000000000711, 0.5000000000000004441 ) ) ;
#6412 = ORIENTED_EDGE ( 'NONE', *, *, #1360, .F. ) ;
#6413 = PLANE ( 'NONE',  #8732 ) ;
#6414 = CARTESIAN_POINT ( 'NONE',  ( -24.00000000000000000, 110.0000000000000000, 30.00000000000000000 ) ) ;
#6415 = CARTESIAN_POINT ( 'NONE',  ( 1.844224359752661968, -38.39960408384397539, 3.000000000000000000 ) ) ;
#6416 = STYLED_ITEM ( 'NONE', ( #4765 ), #16938 ) ;
#6417 = CARTESIAN_POINT ( 'NONE',  ( -2.066987300000000971, 63.14382582708704916, 45.00000000109247367 ) ) ;
#6418 = ADVANCED_FACE ( 'NONE', ( #9243 ), #1871, .F. ) ;
#6419 = ADVANCED_FACE ( 'NONE', ( #16801, #15324, #16898 ), #1904, .F. ) ;
#6420 = CARTESIAN_POINT ( 'NONE',  ( -1.040834085586084257E-14, 29.74264068711926257, 56.74264068711929809 ) ) ;
#6421 = CARTESIAN_POINT ( 'NONE',  ( -7.499999999999994671, -26.00000000000000355, 12.50000000000000000 ) ) ;
#6422 = CARTESIAN_POINT ( 'NONE',  ( -4.999999999999996447, -32.00000000000000000, 4.500000000000000888 ) ) ;
#6423 = EDGE_LOOP ( 'NONE', ( #15863, #4103, #19166, #15389 ) ) ;
#6424 = EDGE_CURVE ( 'NONE', #2590, #18664, #1996, .T. ) ;
#6425 = CARTESIAN_POINT ( 'NONE',  ( -10.58745947852649927, -21.64274437364853654, 15.63867750791695777 ) ) ;
#6426 = AXIS2_PLACEMENT_3D ( 'NONE', #8096, #17110, #3675 ) ;
#6427 = CARTESIAN_POINT ( 'NONE',  ( 2.500000000000002220, 62.96446609406726935, 46.45000000218495018 ) ) ;
#6428 = CARTESIAN_POINT ( 'NONE',  ( -19.99999999999999645, -24.16482700510261949, 20.67382249208304401 ) ) ;
#6429 = DIRECTION ( 'NONE',  ( -1.000000000000000000, 0.000000000000000000, 0.000000000000000000 ) ) ;
#6430 = CARTESIAN_POINT ( 'NONE',  ( -11.21908421996108629, -20.46040770435011069, 15.41992750791695954 ) ) ;
#6431 = PLANE ( 'NONE',  #2339 ) ;
#6432 = CARTESIAN_POINT ( 'NONE',  ( -17.64274437364855430, -28.24771351637087236, 23.07617750791695954 ) ) ;
#6433 = DIRECTION ( 'NONE',  ( 0.000000000000000000, 0.000000000000000000, -1.000000000000000000 ) ) ;
#6434 = CARTESIAN_POINT ( 'NONE',  ( -17.64274437364858983, -19.75228648362910633, 21.54882249208304401 ) ) ;
#6435 = EDGE_CURVE ( 'NONE', #17858, #6216, #12469, .T. ) ;
#6436 = CARTESIAN_POINT ( 'NONE',  ( 2.066987300000002303, 63.14382582708705627, 48.50000000109246656 ) ) ;
#6437 = DIRECTION ( 'NONE',  ( -0.000000000000000000, -0.000000000000000000, -1.000000000000000000 ) ) ;
#6438 = LINE ( 'NONE', #12406, #2539 ) ;
#6439 = VECTOR ( 'NONE', #3148, 1000.000000000000000 ) ;
#6440 = CARTESIAN_POINT ( 'NONE',  ( -14.99999999999999645, 73.00000000000001421, 23.99999999999997868 ) ) ;
#6441 = CARTESIAN_POINT ( 'NONE',  ( 2.066987300000001415, 64.00000000000000000, 47.75000000109246656 ) ) ;
#6442 = CARTESIAN_POINT ( 'NONE',  ( -40.00000000000000000, 53.00000000000000711, 30.00000000000000000 ) ) ;
#6443 = EDGE_LOOP ( 'NONE', ( #7055, #10895, #11146, #17516 ) ) ;
#6444 = ORIENTED_EDGE ( 'NONE', *, *, #7742, .T. ) ;
#6445 = CARTESIAN_POINT ( 'NONE',  ( -16.71081734191520596, -31.04416526290808065, 30.08007249208304046 ) ) ;
#6446 =( LENGTH_UNIT ( ) NAMED_UNIT ( * ) SI_UNIT ( .MILLI., .METRE. ) );
#6447 = CARTESIAN_POINT ( 'NONE',  ( -19.24771351637086880, -26.64274437364857206, 4.486322492083041347 ) ) ;
#6448 = ORIENTED_EDGE ( 'NONE', *, *, #9630, .T. ) ;
#6449 = CARTESIAN_POINT ( 'NONE',  ( -17.31681416490115311, -26.07549068051209318, 33.79492750791695954 ) ) ;
#6450 = LINE ( 'NONE', #6547, #16462 ) ;
#6451 = CARTESIAN_POINT ( 'NONE',  ( -14.83517299489734853, -30.99999999999998224, 24.61132249208304046 ) ) ;
#6452 = AXIS2_PLACEMENT_3D ( 'NONE', #2956, #5713, #13434 ) ;
#6453 = VECTOR ( 'NONE', #7925, 1000.000000000000000 ) ;
#6454 = CARTESIAN_POINT ( 'NONE',  ( -0.8561741729129461742, 66.06698729999999387, 47.80000000109247082 ) ) ;
#6455 = CARTESIAN_POINT ( 'NONE',  ( -1.461580736456473906, 65.46158073645646880, 47.05000000109247082 ) ) ;
#6456 = ORIENTED_EDGE ( 'NONE', *, *, #16510, .T. ) ;
#6457 = ORIENTED_EDGE ( 'NONE', *, *, #15060, .F. ) ;
#6458 = CARTESIAN_POINT ( 'NONE',  ( 0.000000000000000000, 64.00000000000000000, 49.99999999999999289 ) ) ;
#6459 = CYLINDRICAL_SURFACE ( 'NONE', #17272, 4.000000000000001776 ) ;
#6460 = CARTESIAN_POINT ( 'NONE',  ( -2.066987300000001415, 64.00000000000000000, 49.55000000109247082 ) ) ;
#6461 = DIRECTION ( 'NONE',  ( 0.000000000000000000, -0.000000000000000000, 1.000000000000000000 ) ) ;
#6462 = CARTESIAN_POINT ( 'NONE',  ( -2.066987300000001415, 64.00000000000000000, 45.75000000109247367 ) ) ;
#6463 = CARTESIAN_POINT ( 'NONE',  ( -40.00000000000000711, 113.0000000000000000, 30.00000000000000000 ) ) ;
#6464 = CIRCLE ( 'NONE', #15842, 1.678500596222258556 ) ;
#6465 = VECTOR ( 'NONE', #5240, 1000.000000000000000 ) ;
#6466 = FACE_OUTER_BOUND ( 'NONE', #6423, .T. ) ;
#6467 = ORIENTED_EDGE ( 'NONE', *, *, #12749, .F. ) ;
#6469 = ORIENTED_EDGE ( 'NONE', *, *, #11513, .F. ) ;
#6468 = VERTEX_POINT ( 'NONE', #12756 ) ;
#6470 = CARTESIAN_POINT ( 'NONE',  ( -12.95952864787955150, -17.04416526290805933, 35.98242750791695244 ) ) ;
#6471 =( NAMED_UNIT ( * ) SI_UNIT ( $, .STERADIAN. ) SOLID_ANGLE_UNIT ( ) );
#6472 = ORIENTED_EDGE ( 'NONE', *, *, #4486, .F. ) ;
#6473 = ORIENTED_EDGE ( 'NONE', *, *, #1969, .T. ) ;
#6474 = CARTESIAN_POINT ( 'NONE',  ( -17.31681416490117087, -21.92450931948788551, 26.58007249208304756 ) ) ;
#6475 = CARTESIAN_POINT ( 'NONE',  ( -20.24501739517664234, -29.00369391078761439, 12.79492750791695599 ) ) ;
#6476 = CARTESIAN_POINT ( 'NONE',  ( -1.461580736456473462, 62.53841926354353120, 48.05000000109247082 ) ) ;
#6477 = LINE ( 'NONE', #8141, #14716 ) ;
#6478 = EDGE_LOOP ( 'NONE', ( #1257, #5893 ) ) ;
#6479 = CARTESIAN_POINT ( 'NONE',  ( -12.92450931948788906, -26.31681416490114245, 21.98242750791695954 ) ) ;
#6480 = VECTOR ( 'NONE', #8529, 1000.000000000000000 ) ;
#6481 =( NAMED_UNIT ( * ) SI_UNIT ( $, .STERADIAN. ) SOLID_ANGLE_UNIT ( ) );
#6482 = VERTEX_POINT ( 'NONE', #11467 ) ;
#6483 = CIRCLE ( 'NONE', #3348, 1.599999999999997202 ) ;
#6484 = DIRECTION ( 'NONE',  ( -7.709882115452476934E-17, 0.000000000000000000, -1.000000000000000000 ) ) ;
#6485 = ORIENTED_EDGE ( 'NONE', *, *, #5935, .T. ) ;
#6486 = CARTESIAN_POINT ( 'NONE',  ( -2.750000000000020872, 118.0000000000000142, 37.49999999999997158 ) ) ;
#6487 = LINE ( 'NONE', #18352, #12527 ) ;
#6488 = DIRECTION ( 'NONE',  ( 0.000000000000000000, -0.000000000000000000, -1.000000000000000000 ) ) ;
#6489 = FACE_BOUND ( 'NONE', #15711, .T. ) ;
#6490 = CARTESIAN_POINT ( 'NONE',  ( 2.066987300000001859, 64.85617417291294373, 49.20000000109247651 ) ) ;
#6491 = CONTEXT_DEPENDENT_SHAPE_REPRESENTATION ( #4445, #13496 ) ;
#6492 = CARTESIAN_POINT ( 'NONE',  ( -1.035533905932738641, 66.50000000000000000, 49.15000000218494591 ) ) ;
#6493 = CARTESIAN_POINT ( 'NONE',  ( 14.99999999999998579, 47.00000000000000711, 20.99999999999997513 ) ) ;
#6494 = EDGE_CURVE ( 'NONE', #15771, #17858, #718, .T. ) ;
#6495 = CARTESIAN_POINT ( 'NONE',  ( -1.530808498934192803E-16, 66.50000000000000000, 49.79999999999999716 ) ) ;
#6496 = DIRECTION ( 'NONE',  ( 0.000000000000000000, -1.287488025362403787E-15, -1.000000000000000000 ) ) ;
#6497 = ORIENTED_EDGE ( 'NONE', *, *, #3754, .T. ) ;
#6499 = EDGE_CURVE ( 'NONE', #4424, #9683, #15805, .T. ) ;
#6498 = CARTESIAN_POINT ( 'NONE',  ( -12.35725562635143682, -19.75228648362908501, 30.95117750791695954 ) ) ;
#6500 = CIRCLE ( 'NONE', #16175, 2.999999999999999112 ) ;
#6501 = CARTESIAN_POINT ( 'NONE',  ( -32.50000000000000000, 47.00000000000000711, -37.50000000000000711 ) ) ;
#6502 = VERTEX_POINT ( 'NONE', #14145 ) ;
#6503 = CARTESIAN_POINT ( 'NONE',  ( -19.95583473709190514, -25.50457296725822687, 36.20507249208303335 ) ) ;
#6504 = EDGE_CURVE ( 'NONE', #11173, #1259, #4235, .T. ) ;
#6505 = CARTESIAN_POINT ( 'NONE',  ( -12.68318583509882380, -26.07549068051207541, 23.95507249208304756 ) ) ;
#6506 = PRESENTATION_STYLE_ASSIGNMENT (( #329 ) ) ;
#6507 = ORIENTED_EDGE ( 'NONE', *, *, #11406, .F. ) ;
#6508 = CARTESIAN_POINT ( 'NONE',  ( -24.00000000000000000, 53.00000000000000711, -50.00000000000000000 ) ) ;
#6509 = ORIENTED_EDGE ( 'NONE', *, *, #5077, .F. ) ;
#6510 = DIRECTION ( 'NONE',  ( 1.000000000000000000, -7.210288835911348201E-15, 7.602811950582247805E-15 ) ) ;
#6511 = CARTESIAN_POINT ( 'NONE',  ( -2.500000000000001776, 64.00000000000000000, 46.00000000000000000 ) ) ;
#6512 = DIRECTION ( 'NONE',  ( 0.000000000000000000, 0.000000000000000000, -1.000000000000000000 ) ) ;
#6513 = FACE_OUTER_BOUND ( 'NONE', #12126, .T. ) ;
#6514 = EDGE_CURVE ( 'NONE', #993, #17457, #14423, .T. ) ;
#6515 = DIRECTION ( 'NONE',  ( 0.000000000000000000, 0.000000000000000000, -1.000000000000000000 ) ) ;
#6516 = CARTESIAN_POINT ( 'NONE',  ( 3.099999999999998757, 0.000000000000000000, -1.600000000000000311 ) ) ;
#6517 = FACE_OUTER_BOUND ( 'NONE', #14290, .T. ) ;
#6518 = VERTEX_POINT ( 'NONE', #11280 ) ;
#6519 = CARTESIAN_POINT ( 'NONE',  ( -9.955834737091912245, -22.82508104294696594, 21.10742750791695599 ) ) ;
#6520 = CARTESIAN_POINT ( 'NONE',  ( 2.500000000000001776, 65.03553390593273775, 46.55000000218494449 ) ) ;
#6521 = CARTESIAN_POINT ( 'NONE',  ( -11.46040770435014977, -20.21908421996103655, 22.64257249208303335 ) ) ;
#6522 = ADVANCED_FACE ( 'NONE', ( #3938 ), #18752, .T. ) ;
#6523 = ADVANCED_FACE ( 'NONE', ( #15998 ), #12848, .T. ) ;
#6524 = DIRECTION ( 'NONE',  ( 0.000000000000000000, -1.000000000000000000, 0.000000000000000000 ) ) ;
#6525 = CARTESIAN_POINT ( 'NONE',  ( -13.49542703274178379, -19.04416526290806289, 14.98242750791695777 ) ) ;
#6526 = EDGE_CURVE ( 'NONE', #3207, #7196, #8541, .T. ) ;
#6527 = CARTESIAN_POINT ( 'NONE',  ( 0.000000000000000000, -1.478016689125442706, 1.843143693225357538E-15 ) ) ;
#6528 = CARTESIAN_POINT ( 'NONE',  ( -14.83517299489739649, -18.99999999999997868, 35.76367750791695954 ) ) ;
#6529 = DIRECTION ( 'NONE',  ( 0.000000000000000000, -0.7071067811865493491, 0.7071067811865457964 ) ) ;
#6530 = CARTESIAN_POINT ( 'NONE',  ( -19.99999999999999645, -24.16482700510261949, 20.67382249208304401 ) ) ;
#6531 = CARTESIAN_POINT ( 'NONE',  ( 0.8561741729129472844, 61.93301270000000613, 47.60000000109246798 ) ) ;
#6532 = CARTESIAN_POINT ( 'NONE',  ( -7.499999999999994671, -38.00000000000000000, 12.50000000000000000 ) ) ;
#6533 = SHAPE_REPRESENTATION ( 'socket head cap screw_iso_ISO 4762 M5 x 8 - 8N', ( #1791 ), #9226 ) ;
#6534 = LINE ( 'NONE', #13778, #14142 ) ;
#6535 = CARTESIAN_POINT ( 'NONE',  ( 3.399999999999996803, 29.47747564417430155, 56.65425233947098604 ) ) ;
#6536 = CARTESIAN_POINT ( 'NONE',  ( 1.461580736456473684, 65.46158073645646880, 47.05000000109247082 ) ) ;
#6537 = CYLINDRICAL_SURFACE ( 'NONE', #11122, 2.499999999999998668 ) ;
#6538 = VECTOR ( 'NONE', #2210, 1000.000000000000000 ) ;
#6539 = ORIENTED_EDGE ( 'NONE', *, *, #11499, .T. ) ;
#6540 = EDGE_LOOP ( 'NONE', ( #16889, #7736, #10864, #16239 ) ) ;
#6541 = CARTESIAN_POINT ( 'NONE',  ( -8.044165262908093084, -21.95952864787946979, 33.58007249208304046 ) ) ;
#6542 = CARTESIAN_POINT ( 'NONE',  ( -18.78091578003892792, -20.46040770435013556, 16.08007249208304046 ) ) ;
#6543 = VERTEX_POINT ( 'NONE', #997 ) ;
#6544 = ADVANCED_FACE ( 'NONE', ( #6973 ), #5140, .T. ) ;
#6545 = CARTESIAN_POINT ( 'NONE',  ( -17.99999999999999645, -23.83517299489736985, 23.95117750791696309 ) ) ;
#6546 = EDGE_CURVE ( 'NONE', #10710, #9506, #9627, .T. ) ;
#6547 = CARTESIAN_POINT ( 'NONE',  ( -32.50000000000000000, 52.00000000000000711, 17.49999999999999645 ) ) ;
#6548 = CARTESIAN_POINT ( 'NONE',  ( -11.35725562635139418, -29.97976432393972601, 13.67382249208304046 ) ) ;
#6549 = AXIS2_PLACEMENT_3D ( 'NONE', #15498, #6585, #12264 ) ;
#6550 = CARTESIAN_POINT ( 'NONE',  ( 0.8561741729129472844, 61.93301270000000613, 47.40000000109247225 ) ) ;
#6551 = DIRECTION ( 'NONE',  ( 0.000000000000000000, 0.000000000000000000, 1.000000000000000000 ) ) ;
#6552 = VERTEX_POINT ( 'NONE', #8173 ) ;
#6553 = VERTEX_POINT ( 'NONE', #17365 ) ;
#6554 = AXIS2_PLACEMENT_3D ( 'NONE', #14639, #18353, #10510 ) ;
#6555 = DIRECTION ( 'NONE',  ( -0.000000000000000000, -0.000000000000000000, -1.000000000000000000 ) ) ;
#6556 = PLANE ( 'NONE',  #7242 ) ;
#6557 = CARTESIAN_POINT ( 'NONE',  ( -1.461580736456473906, 65.46158073645646880, 47.85000000109246798 ) ) ;
#6558 = LINE ( 'NONE', #3606, #10301 ) ;
#6559 = CARTESIAN_POINT ( 'NONE',  ( -2.066987300000001415, 64.00000000000000000, 44.95000000109246940 ) ) ;
#6560 = CARTESIAN_POINT ( 'NONE',  ( 0.000000000000000000, 0.000000000000000000, 0.000000000000000000 ) ) ;
#6561 = VECTOR ( 'NONE', #2992, 1000.000000000000000 ) ;
#6562 = ORIENTED_EDGE ( 'NONE', *, *, #17065, .T. ) ;
#6563 = VERTEX_POINT ( 'NONE', #9811 ) ;
#6564 = CARTESIAN_POINT ( 'NONE',  ( -9.020235676060220698, -27.64274437364852588, 32.26367750791695244 ) ) ;
#6565 = AXIS2_PLACEMENT_3D ( 'NONE', #17973, #11782, #8944 ) ;
#6566 = CARTESIAN_POINT ( 'NONE',  ( -14.99999999999999645, 3.000000000000000000, 23.99999999999997868 ) ) ;
#6567 = ORIENTED_EDGE ( 'NONE', *, *, #18266, .T. ) ;
#6568 = VECTOR ( 'NONE', #7836, 1000.000000000000000 ) ;
#6570 = VERTEX_POINT ( 'NONE', #2373 ) ;
#6569 = EDGE_LOOP ( 'NONE', ( #4392, #6761, #2820, #1344 ) ) ;
#6571 = ADVANCED_FACE ( 'NONE', ( #11187 ), #12940, .T. ) ;
#6572 = CARTESIAN_POINT ( 'NONE',  ( -16.64274437364858272, -21.48433729119797420, 32.04882249208304756 ) ) ;
#6573 = CARTESIAN_POINT ( 'NONE',  ( -20.24501739517664234, -29.00369391078761439, 23.29492750791695599 ) ) ;
#6574 = LINE ( 'NONE', #3623, #14156 ) ;
#6575 = CARTESIAN_POINT ( 'NONE',  ( 2.066987300000001415, 64.00000000000000000, 48.35000000109246798 ) ) ;
#6576 = LINE ( 'NONE', #1967, #15031 ) ;
#6577 = ORIENTED_EDGE ( 'NONE', *, *, #6199, .T. ) ;
#6578 = CARTESIAN_POINT ( 'NONE',  ( -14.83517299489738761, -20.99999999999997513, 25.26367750791696309 ) ) ;
#6579 = AXIS2_PLACEMENT_3D ( 'NONE', #12751, #17273, #3839 ) ;
#6580 = FILL_AREA_STYLE ('',( #15588 ) ) ;
#6581 = ORIENTED_EDGE ( 'NONE', *, *, #8836, .T. ) ;
#6582 = CARTESIAN_POINT ( 'NONE',  ( 1.300000000000000044, -0.7390083445627200209, 1.280000000000001137 ) ) ;
#6583 = ORIENTED_EDGE ( 'NONE', *, *, #13319, .F. ) ;
#6584 = DIRECTION ( 'NONE',  ( -0.000000000000000000, 1.000000000000000000, -0.000000000000000000 ) ) ;
#6585 = DIRECTION ( 'NONE',  ( 0.000000000000000000, 0.8660254037844379305, -0.5000000000000014433 ) ) ;
#6586 = FACE_BOUND ( 'NONE', #16261, .T. ) ;
#6587 = DIRECTION ( 'NONE',  ( -1.000000000000000000, 0.000000000000000000, -0.000000000000000000 ) ) ;
#6588 = AXIS2_PLACEMENT_3D ( 'NONE', #18765, #914, #5622 ) ;
#6589 = CARTESIAN_POINT ( 'NONE',  ( 2.066987300000002303, 63.14382582708705627, 49.10000000109246088 ) ) ;
#6590 = CARTESIAN_POINT ( 'NONE',  ( 2.066987300000001859, 63.14382582708704916, 46.90000000109247225 ) ) ;
#6591 = DIRECTION ( 'NONE',  ( 1.000000000000000000, -0.000000000000000000, -0.000000000000000000 ) ) ;
#6592 = LINE ( 'NONE', #413, #3661 ) ;
#6593 = CIRCLE ( 'NONE', #12523, 2.500000000000002220 ) ;
#6594 = FACE_OUTER_BOUND ( 'NONE', #1846, .T. ) ;
#6595 = VERTEX_POINT ( 'NONE', #15715 ) ;
#6596 = CARTESIAN_POINT ( 'NONE',  ( -13.49542703274178379, -19.04416526290806289, 30.73242750791695599 ) ) ;
#6597 = LINE ( 'NONE', #18564, #10841 ) ;
#6598 = ADVANCED_FACE ( 'NONE', ( #18849 ), #5504, .T. ) ;
#6599 = ORIENTED_EDGE ( 'NONE', *, *, #4533, .T. ) ;
#6600 = VECTOR ( 'NONE', #10132, 1000.000000000000000 ) ;
#6601 = EDGE_CURVE ( 'NONE', #185, #7469, #17458, .T. ) ;
#6602 = CARTESIAN_POINT ( 'NONE',  ( -12.64274437364858628, -19.58745947852646552, 38.17382249208304046 ) ) ;
#6603 = VECTOR ( 'NONE', #11962, 1000.000000000000114 ) ;
#6604 = CARTESIAN_POINT ( 'NONE',  ( -14.03132541760400009, -26.95583473709189448, 34.89257249208305467 ) ) ;
#6605 = CARTESIAN_POINT ( 'NONE',  ( -31.74999999999995737, 0.000000000000000000, 4.250000000000000000 ) ) ;
#6606 = ORIENTED_EDGE ( 'NONE', *, *, #12234, .T. ) ;
#6607 = AXIS2_PLACEMENT_3D ( 'NONE', #1696, #3167, #5912 ) ;
#6608 = LINE ( 'NONE', #7886, #18481 ) ;
#6609 = ORIENTED_EDGE ( 'NONE', *, *, #6762, .T. ) ;
#6610 = CARTESIAN_POINT ( 'NONE',  ( -2.500000000000001776, 64.00000000000000000, 48.50000000218494023 ) ) ;
#6611 = CARTESIAN_POINT ( 'NONE',  ( -25.00000000000000000, 113.0000000000000000, 30.00000000000000000 ) ) ;
#6612 = VECTOR ( 'NONE', #7457, 1000.000000000000000 ) ;
#6613 = VECTOR ( 'NONE', #13931, 1000.000000000000000 ) ;
#6614 = PLANE ( 'NONE',  #4851 ) ;
#6615 = PLANE ( 'NONE',  #18526 ) ;
#6616 = CARTESIAN_POINT ( 'NONE',  ( -7.999999999999986677, 60.00000000000000711, 69.99999999999998579 ) ) ;
#6617 = CARTESIAN_POINT ( 'NONE',  ( 5.199999999999996625, 0.000000000000000000, 0.000000000000000000 ) ) ;
#6618 = ORIENTED_EDGE ( 'NONE', *, *, #11880, .F. ) ;
#6619 = VECTOR ( 'NONE', #3660, 1000.000000000000000 ) ;
#6620 = CARTESIAN_POINT ( 'NONE',  ( -17.64274437364855430, -28.24771351637087236, 28.32617750791695954 ) ) ;
#6621 = CARTESIAN_POINT ( 'NONE',  ( 1.035533905932738197, 66.50000000000000000, 46.65000000218494591 ) ) ;
#6622 = ADVANCED_FACE ( 'NONE', ( #2560 ), #14516, .T. ) ;
#6623 = CARTESIAN_POINT ( 'NONE',  ( -14.83517299489735741, -28.99999999999998224, 24.61132249208304401 ) ) ;
#6624 = VECTOR ( 'NONE', #532, 1000.000000000000000 ) ;
#6625 = CARTESIAN_POINT ( 'NONE',  ( -19.99999999999999645, -32.00000000000000711, 1.500000000000000000 ) ) ;
#6626 = CARTESIAN_POINT ( 'NONE',  ( -20.04416526290808065, -25.17491895705300209, 18.48242750791695954 ) ) ;
#6627 = VECTOR ( 'NONE', #10753, 1000.000000000000000 ) ;
#6628 = DIRECTION ( 'NONE',  ( 1.000000000000000000, -0.000000000000000000, -0.000000000000000000 ) ) ;
#6629 = CARTESIAN_POINT ( 'NONE',  ( -11.46040770435012490, -27.78091578003888173, 27.23242750791695599 ) ) ;
#6630 = CARTESIAN_POINT ( 'NONE',  ( -1.040834085586084257E-14, 29.74264068711925901, 56.74264068711929809 ) ) ;
#6631 = CARTESIAN_POINT ( 'NONE',  ( -14.83517299489735741, -28.99999999999998224, 24.61132249208304401 ) ) ;
#6632 = CARTESIAN_POINT ( 'NONE',  ( 2.066987300000001415, 64.00000000000000000, 45.35000000109246798 ) ) ;
#6633 = DIRECTION ( 'NONE',  ( 0.7071067811865561215, 0.4999999999999953926, -0.4999999999999925060 ) ) ;
#6634 = DIRECTION ( 'NONE',  ( 1.000000000000000000, 0.000000000000000000, 0.000000000000000000 ) ) ;
#6635 = VECTOR ( 'NONE', #16829, 1000.000000000000000 ) ;
#6636 = CARTESIAN_POINT ( 'NONE',  ( -41.00000000000000711, 110.0000000000000000, 21.00000000000000000 ) ) ;
#6637 = CARTESIAN_POINT ( 'NONE',  ( 0.8561741729129460632, 66.06698729999999387, 47.10000000109246798 ) ) ;
#6638 = CARTESIAN_POINT ( 'NONE',  ( -0.1250000000000104083, 27.16170093578836031, 58.97002704785691662 ) ) ;
#6639 = EDGE_CURVE ( 'NONE', #19248, #1662, #17859, .T. ) ;
#6640 = VERTEX_POINT ( 'NONE', #8833 ) ;
#6641 = EDGE_CURVE ( 'NONE', #8073, #16874, #10391, .T. ) ;
#6642 = CARTESIAN_POINT ( 'NONE',  ( -12.95952864787948755, -30.95583473709188382, 29.64257249208304401 ) ) ;
#6643 = CARTESIAN_POINT ( 'NONE',  ( -50.00000000000001421, 33.00000000000000000, 44.99999999999999289 ) ) ;
#6644 = CARTESIAN_POINT ( 'NONE',  ( -14.36097942780923731, -27.04416526290806999, 27.66992750791696665 ) ) ;
#6645 = CARTESIAN_POINT ( 'NONE',  ( -2.500000000000001776, 64.00000000000000000, 49.99999999999999289 ) ) ;
#6646 = CARTESIAN_POINT ( 'NONE',  ( -11.35725562635139418, -29.97976432393972601, 24.17382249208304046 ) ) ;
#6647 = CARTESIAN_POINT ( 'NONE',  ( -2.066987300000001415, 64.00000000000000000, 47.15000000109247225 ) ) ;
#6648 = ORIENTED_EDGE ( 'NONE', *, *, #14320, .F. ) ;
#6649 = ORIENTED_EDGE ( 'NONE', *, *, #3507, .F. ) ;
#6650 = VECTOR ( 'NONE', #14651, 1000.000000000000000 ) ;
#6651 = CARTESIAN_POINT ( 'NONE',  ( -15.20357423236093375, -43.78611686177728046, 3.000000000000000000 ) ) ;
#6652 = CARTESIAN_POINT ( 'NONE',  ( 4.000000000000003553, 47.00000000000000711, 34.99999999999999289 ) ) ;
#6653 = CARTESIAN_POINT ( 'NONE',  ( 50.00000000000000000, 118.0000000000000142, -60.00000000000000000 ) ) ;
#6654 = CYLINDRICAL_SURFACE ( 'NONE', #12806, 2.500000000000001776 ) ;
#6655 = CARTESIAN_POINT ( 'NONE',  ( -1.265664690411616068E-16, 66.06698730000000808, 45.55000000109246372 ) ) ;
#6656 = DIRECTION ( 'NONE',  ( -0.000000000000000000, -0.7071067811865456854, -0.7071067811865494601 ) ) ;
#6657 = ADVANCED_BREP_SHAPE_REPRESENTATION ( '', ( #10426, #1791 ), #1419 ) ;
#6658 = EDGE_CURVE ( 'NONE', #14054, #15935, #17655, .T. ) ;
#6659 = CARTESIAN_POINT ( 'NONE',  ( 0.1249999999999895917, 25.46464466094064250, 60.66708332270462734 ) ) ;
#6660 = VERTEX_POINT ( 'NONE', #19133 ) ;
#6661 = ORIENTED_EDGE ( 'NONE', *, *, #3502, .T. ) ;
#6662 = CARTESIAN_POINT ( 'NONE',  ( -16.71081734191527346, -16.95583473709190159, 30.29492750791696665 ) ) ;
#6663 = VERTEX_POINT ( 'NONE', #7162 ) ;
#6665 = ORIENTED_EDGE ( 'NONE', *, *, #14433, .T. ) ;
#6664 = ORIENTED_EDGE ( 'NONE', *, *, #1001, .F. ) ;
#6666 = CARTESIAN_POINT ( 'NONE',  ( -17.99999999999999645, -24.16482700510260173, 25.92382249208304756 ) ) ;
#6667 = ADVANCED_FACE ( 'NONE', ( #16385 ), #4139, .F. ) ;
#6668 = CARTESIAN_POINT ( 'NONE',  ( -11.35725562635144925, -18.02023567606020293, 20.45117750791695954 ) ) ;
#6669 = CLOSED_SHELL ( 'NONE', ( #13824, #11391, #3292, #14301, #3077, #5675, #11159, #2071, #10716, #4333, #15355, #15726, #12386, #5481, #17441, #14266, #5830, #12998, #17418, #3038, #1489, #10349, #10471, #13316, #14310, #6419, #9155, #19198, #6523, #13048, #6888, #1217, #16857, #18862, #4448, #11307, #6327, #17665, #102, #18017, #2401, #10217, #17746, #2586, #13047, #1990, #17157, #5119, #9590, #12383 ) ) ;
#6670 = FACE_BOUND ( 'NONE', #16051, .T. ) ;
#6671 = CARTESIAN_POINT ( 'NONE',  ( -1.035533905932738863, 61.50000000000000000, 47.05000000218494449 ) ) ;
#6672 = CARTESIAN_POINT ( 'NONE',  ( -7.999999999999986677, 68.00000000000000000, 45.00000000000000000 ) ) ;
#6673 = VERTEX_POINT ( 'NONE', #1291 ) ;
#6674 = CARTESIAN_POINT ( 'NONE',  ( -17.68048971390461688, -25.35725562635141372, 28.76367750791696309 ) ) ;
#6675 = DIRECTION ( 'NONE',  ( 0.000000000000000000, 0.000000000000000000, -1.000000000000000000 ) ) ;
#6676 = ORIENTED_EDGE ( 'NONE', *, *, #18362, .T. ) ;
#6677 = DIRECTION ( 'NONE',  ( 0.000000000000000000, -0.7071067811865457964, -0.7071067811865492381 ) ) ;
#6678 = ORIENTED_EDGE ( 'NONE', *, *, #15149, .T. ) ;
#6679 = LINE ( 'NONE', #8058, #7890 ) ;
#6680 = PLANE ( 'NONE',  #6549 ) ;
#6681 = DIRECTION ( 'NONE',  ( 0.000000000000000000, 0.000000000000000000, -1.000000000000000000 ) ) ;
#6682 = CARTESIAN_POINT ( 'NONE',  ( 3.796994071234847710E-16, 61.93301269999999903, 48.95000000109246940 ) ) ;
#6683 = EDGE_CURVE ( 'NONE', #19310, #8146, #2949, .T. ) ;
#6684 = LINE ( 'NONE', #14026, #6613 ) ;
#6685 = DIRECTION ( 'NONE',  ( 0.000000000000000000, 0.7071067811865456854, 0.7071067811865494601 ) ) ;
#6686 = CARTESIAN_POINT ( 'NONE',  ( 2.492551403682577771, 31.20336399182262710, 54.92836399182266405 ) ) ;
#6687 = ORIENTED_EDGE ( 'NONE', *, *, #12110, .F. ) ;
#6688 = CARTESIAN_POINT ( 'NONE',  ( -19.24771351637089367, -21.35725562635142438, 29.63867750791695599 ) ) ;
#6689 = DIRECTION ( 'NONE',  ( 0.7071067811865512365, 0.4999999999999988898, -0.4999999999999959477 ) ) ;
#6690 = ORIENTED_EDGE ( 'NONE', *, *, #9803, .T. ) ;
#6691 = CARTESIAN_POINT ( 'NONE',  ( -17.64274437364858983, -19.75228648362910633, 26.79882249208304401 ) ) ;
#6692 = CARTESIAN_POINT ( 'NONE',  ( 4.592425496802577917E-16, 61.50000000000000000, 45.39999999999999858 ) ) ;
#6693 = PRODUCT_DEFINITION ( 'UNKNOWN', '', #17687, #16098 ) ;
#6694 = CARTESIAN_POINT ( 'NONE',  ( -14.36097942780925685, -20.95583473709189093, 27.45507249208304756 ) ) ;
#6695 = CYLINDRICAL_SURFACE ( 'NONE', #15978, 2.999999999999999112 ) ;
#6696 = ORIENTED_EDGE ( 'NONE', *, *, #9412, .F. ) ;
#6697 = DIRECTION ( 'NONE',  ( 1.156482317317871478E-16, -1.000000000000000000, 0.000000000000000000 ) ) ;
#6698 = VERTEX_POINT ( 'NONE', #13234 ) ;
#6699 = DIRECTION ( 'NONE',  ( 0.000000000000000000, -0.5000000000000013323, -0.8660254037844380415 ) ) ;
#6700 = CARTESIAN_POINT ( 'NONE',  ( 1.767766952966369987, 65.76776695296638309, 45.80000000218493739 ) ) ;
#6701 = PLANE ( 'NONE',  #136 ) ;
#6702 = CARTESIAN_POINT ( 'NONE',  ( -25.00000000000000000, 53.00000000000000711, -44.00000000000000000 ) ) ;
#6703 = CARTESIAN_POINT ( 'NONE',  ( 41.00000000000000000, 47.00000000000000711, 30.00000000000000000 ) ) ;
#6704 = EDGE_LOOP ( 'NONE', ( #19311, #1947, #12918, #12996 ) ) ;
#6705 = CARTESIAN_POINT ( 'NONE',  ( -12.35725562635143682, -19.75228648362908501, 30.95117750791695954 ) ) ;
#6706 = EDGE_CURVE ( 'NONE', #16534, #2938, #1587, .T. ) ;
#6707 = CARTESIAN_POINT ( 'NONE',  ( -1.265664690411616068E-16, 66.06698730000000808, 48.55000000109247082 ) ) ;
#6708 = CARTESIAN_POINT ( 'NONE',  ( -16.50457296725825174, -19.04416526290807354, 27.01757249208304046 ) ) ;
#6709 = COLOUR_RGB ( '', 0.40784314, 0.44705882, 0.49803922) ;
#6710 = CARTESIAN_POINT ( 'NONE',  ( 0.000000000000000000, 64.00000000000000000, 49.99999999999999289 ) ) ;
#6711 = CARTESIAN_POINT ( 'NONE',  ( -15.16482700510259640, -28.99999999999998224, 27.88867750791695954 ) ) ;
#6712 = DIRECTION ( 'NONE',  ( -1.000000000000000000, 0.000000000000000000, 0.000000000000000000 ) ) ;
#6713 = CARTESIAN_POINT ( 'NONE',  ( -15.16482700510259640, -28.99999999999998224, 38.38867750791695954 ) ) ;
#6714 = LINE ( 'NONE', #5343, #5301 ) ;
#6715 = CARTESIAN_POINT ( 'NONE',  ( -17.64274437364858983, -19.75228648362910633, 26.79882249208304401 ) ) ;
#6716 = CARTESIAN_POINT ( 'NONE',  ( 0.8561741729129472844, 61.93301270000000613, 45.20000000109248361 ) ) ;
#6717 = DIRECTION ( 'NONE',  ( 1.000000000000000000, -0.000000000000000000, -0.000000000000000000 ) ) ;
#6718 = PLANE ( 'NONE',  #4768 ) ;
#6719 = CARTESIAN_POINT ( 'NONE',  ( 2.500000000000001776, 64.00000000000000000, 49.60000000000000142 ) ) ;
#6720 = EDGE_CURVE ( 'NONE', #3232, #13613, #10189, .T. ) ;
#6721 = ADVANCED_FACE ( 'NONE', ( #7560 ), #6000, .F. ) ;
#6722 = CARTESIAN_POINT ( 'NONE',  ( -0.1250000000000104083, 33.66708332270461312, 52.46464466094069934 ) ) ;
#6723 = VECTOR ( 'NONE', #17999, 1000.000000000000000 ) ;
#6724 = ORIENTED_EDGE ( 'NONE', *, *, #17019, .T. ) ;
#6725 = EDGE_CURVE ( 'NONE', #16897, #13230, #3153, .T. ) ;
#6726 = SURFACE_STYLE_USAGE ( .BOTH. , #3788 ) ;
#6727 = CARTESIAN_POINT ( 'NONE',  ( 2.066987300000001415, 64.00000000000000000, 46.75000000109247367 ) ) ;
#6728 = CARTESIAN_POINT ( 'NONE',  ( -13.35725562635142794, -21.48433729119796709, 30.95117750791695954 ) ) ;
#6729 = CARTESIAN_POINT ( 'NONE',  ( -32.50000000000002132, -6.000000000000000000, -42.50000000000001421 ) ) ;
#6730 = EDGE_CURVE ( 'NONE', #576, #8618, #8724, .T. ) ;
#6731 = CARTESIAN_POINT ( 'NONE',  ( -9.020235676060250896, -20.35725562635137820, 38.61132249208304046 ) ) ;
#6732 = CARTESIAN_POINT ( 'NONE',  ( -2.066987300000001415, 64.00000000000000000, 45.55000000109246372 ) ) ;
#6733 = VERTEX_POINT ( 'NONE', #14713 ) ;
#6734 = CARTESIAN_POINT ( 'NONE',  ( -25.00000000000000711, 53.00000000000000711, -45.00000000000000000 ) ) ;
#6735 = CARTESIAN_POINT ( 'NONE',  ( 11.00000000000000355, 0.000000000000000000, 1.219500000000000028 ) ) ;
#6736 = CARTESIAN_POINT ( 'NONE',  ( 0.8561741729129471734, 61.93301270000000613, 45.80000000109246372 ) ) ;
#6737 = DIRECTION ( 'NONE',  ( -0.000000000000000000, -0.000000000000000000, -1.000000000000000000 ) ) ;
#6738 = ADVANCED_FACE ( 'NONE', ( #5797 ), #11760, .T. ) ;
#6739 = CARTESIAN_POINT ( 'NONE',  ( -1.035533905932738641, 66.50000000000000000, 49.85000000000000853 ) ) ;
#6740 = DIRECTION ( 'NONE',  ( 0.000000000000000000, 0.000000000000000000, 1.000000000000000000 ) ) ;
#6741 = CARTESIAN_POINT ( 'NONE',  ( -2.500000000000001776, 64.00000000000000000, 47.59999999999999432 ) ) ;
#6742 = ORIENTED_EDGE ( 'NONE', *, *, #17824, .T. ) ;
#6743 = EDGE_CURVE ( 'NONE', #16834, #4224, #10286, .T. ) ;
#6744 = VERTEX_POINT ( 'NONE', #1387 ) ;
#6745 = CARTESIAN_POINT ( 'NONE',  ( -11.64274437364854187, -30.14459132904234195, 27.45117750791696309 ) ) ;
#6746 = VECTOR ( 'NONE', #2629, 1000.000000000000000 ) ;
#6747 =( NAMED_UNIT ( * ) PLANE_ANGLE_UNIT ( ) SI_UNIT ( $, .RADIAN. ) );
#6748 = VERTEX_POINT ( 'NONE', #13332 ) ;
#6749 = AXIS2_PLACEMENT_3D ( 'NONE', #747, #4885, #558 ) ;
#6751 = ORIENTED_EDGE ( 'NONE', *, *, #14501, .F. ) ;
#6750 = EDGE_LOOP ( 'NONE', ( #7814, #10770, #16833, #12425 ) ) ;
#6752 = CARTESIAN_POINT ( 'NONE',  ( -17.07549068051208963, -26.31681416490115311, 30.51757249208304756 ) ) ;
#6753 = CARTESIAN_POINT ( 'NONE',  ( -12.95952864787955150, -17.04416526290805933, 35.98242750791695244 ) ) ;
#6754 =( BOUNDED_CURVE ( )  B_SPLINE_CURVE ( 2, ( #9740, #11585, #18869, #2477, #17383, #6805, #1107, #3956, #13052 ),
 .UNSPECIFIED., .F., .F. ) 
 B_SPLINE_CURVE_WITH_KNOTS ( ( 3, 2, 2, 2, 3 ),
 ( 0.4999999999999999445, 0.5178571428571427937, 0.5357142857142855874, 0.5535714285714283811, 0.5714285714285711748 ),
 .UNSPECIFIED. ) 
 CURVE ( )  GEOMETRIC_REPRESENTATION_ITEM ( )  RATIONAL_B_SPLINE_CURVE ( ( 1.000000000000000222, 0.9238795325112865164, 1.000000000000000000, 0.9238795325112867385, 1.000000000000000000, 0.9238795325112867385, 1.000000000000000000, 0.9238795325112877377, 0.9999999999999990008 ) ) 
 REPRESENTATION_ITEM ( '' )  );
#6755 = FACE_BOUND ( 'NONE', #3811, .T. ) ;
#6756 = CARTESIAN_POINT ( 'NONE',  ( 1.035533905932739751, 61.50000000000000000, 48.75000000218494023 ) ) ;
#6757 = PLANE ( 'NONE',  #15338 ) ;
#6758 = ORIENTED_EDGE ( 'NONE', *, *, #7372, .F. ) ;
#6759 = CARTESIAN_POINT ( 'NONE',  ( -14.36097942780923731, -27.04416526290806999, 32.91992750791696665 ) ) ;
#6760 = FACE_OUTER_BOUND ( 'NONE', #10102, .T. ) ;
#6761 = ORIENTED_EDGE ( 'NONE', *, *, #510, .T. ) ;
#6762 = EDGE_CURVE ( 'NONE', #6468, #9777, #14918, .T. ) ;
#6763 = EDGE_CURVE ( 'NONE', #13282, #4488, #16485, .T. ) ;
#6764 = CARTESIAN_POINT ( 'NONE',  ( -25.00000000000000711, 53.00000000000000711, -37.50000000000000711 ) ) ;
#6765 = EDGE_LOOP ( 'NONE', ( #9879, #3809, #13940, #1777 ) ) ;
#6766 = CARTESIAN_POINT ( 'NONE',  ( 32.49999999999998579, -6.000000000000000000, 24.99999999999998579 ) ) ;
#6767 = DIRECTION ( 'NONE',  ( -1.000000000000000000, 0.000000000000000000, 0.000000000000000000 ) ) ;
#6768 = LINE ( 'NONE', #6852, #5617 ) ;
#6769 = EDGE_CURVE ( 'NONE', #3230, #9690, #12, .T. ) ;
#6770 = VECTOR ( 'NONE', #7641, 1000.000000000000114 ) ;
#6771 = CARTESIAN_POINT ( 'NONE',  ( -1.461580736456473906, 65.46158073645646880, 44.65000000109246514 ) ) ;
#6772 = EDGE_CURVE ( 'NONE', #5165, #17673, #19033, .T. ) ;
#6773 = CARTESIAN_POINT ( 'NONE',  ( 3.796994071234847710E-16, 61.93301269999999903, 48.35000000109246798 ) ) ;
#6774 = CARTESIAN_POINT ( 'NONE',  ( 2.500000000000001776, 64.00000000000000000, 49.99999999999999289 ) ) ;
#6775 = DIRECTION ( 'NONE',  ( -1.000000000000000000, 7.210288835911348201E-15, -7.602811950582247805E-15 ) ) ;
#6776 = CARTESIAN_POINT ( 'NONE',  ( -0.08332044287239959157, 25.64046917798804515, 60.84354269072931487 ) ) ;
#6777 = ORIENTED_EDGE ( 'NONE', *, *, #12943, .T. ) ;
#6778 = ORIENTED_EDGE ( 'NONE', *, *, #18605, .F. ) ;
#6779 = CARTESIAN_POINT ( 'NONE',  ( -16.50457296725820555, -28.95583473709189448, 33.35742750791695954 ) ) ;
#6780 = CARTESIAN_POINT ( 'NONE',  ( -37.50000000000002132, -6.000000000000000000, 44.99999999999997868 ) ) ;
#6781 = ORIENTED_EDGE ( 'NONE', *, *, #8780, .T. ) ;
#6782 = CARTESIAN_POINT ( 'NONE',  ( -10.04416526290808953, -22.49542703274172695, 28.33007249208304401 ) ) ;
#6783 = VECTOR ( 'NONE', #15510, 1000.000000000000000 ) ;
#6784 = COLOUR_RGB ( '', 0.66274510, 0.83137255, 0.94901961) ;
#6785 = DIRECTION ( 'NONE',  ( 0.000000000000000000, 1.000000000000000000, 0.000000000000000000 ) ) ;
#6786 = EDGE_CURVE ( 'NONE', #13006, #17737, #12128, .T. ) ;
#6787 = CARTESIAN_POINT ( 'NONE',  ( -17.31681416490117087, -21.92450931948788551, 37.08007249208304756 ) ) ;
#6788 = FACE_OUTER_BOUND ( 'NONE', #14972, .T. ) ;
#6789 = ORIENTED_EDGE ( 'NONE', *, *, #8293, .F. ) ;
#6790 = FACE_OUTER_BOUND ( 'NONE', #7339, .T. ) ;
#6791 = VERTEX_POINT ( 'NONE', #7763 ) ;
#6792 = CARTESIAN_POINT ( 'NONE',  ( -1.767766952966370209, 65.76776695296638309, 45.20000000218494307 ) ) ;
#6793 = CARTESIAN_POINT ( 'NONE',  ( -5.800000000000006928, 29.47747564417435484, 56.65425233947093631 ) ) ;
#6794 = DIRECTION ( 'NONE',  ( 1.000000000000000000, 0.000000000000000000, 0.000000000000000000 ) ) ;
#6795 = STYLED_ITEM ( 'NONE', ( #2420 ), #11089 ) ;
#6796 = MECHANICAL_DESIGN_GEOMETRIC_PRESENTATION_REPRESENTATION (  '', ( #17732 ), #17748 ) ;
#6797 = CARTESIAN_POINT ( 'NONE',  ( -24.00000000000000711, 53.00000000000000711, 26.50000000000000000 ) ) ;
#6798 = FACE_OUTER_BOUND ( 'NONE', #11937, .T. ) ;
#6799 = DIRECTION ( 'NONE',  ( 1.000000000000000000, 0.000000000000000000, 0.000000000000000000 ) ) ;
#6800 = ORIENTED_EDGE ( 'NONE', *, *, #5604, .F. ) ;
#6801 = CARTESIAN_POINT ( 'NONE',  ( -17.35725562635144215, -19.58745947852648683, 35.32617750791695954 ) ) ;
#6802 = EDGE_CURVE ( 'NONE', #12630, #5173, #15377, .T. ) ;
#6803 = CARTESIAN_POINT ( 'NONE',  ( -1.461580736456473462, 62.53841926354353120, 46.45000000109246940 ) ) ;
#6804 = CARTESIAN_POINT ( 'NONE',  ( -15.16482700510263371, -18.99999999999997868, 32.48632249208304046 ) ) ;
#6805 = CARTESIAN_POINT ( 'NONE',  ( -1.035533905932738863, 61.50000000000000000, 46.25000000218494733 ) ) ;
#6806 = CARTESIAN_POINT ( 'NONE',  ( -16.17491895705301275, -18.95583473709189803, 25.04492750791695954 ) ) ;
#6807 = DIRECTION ( 'NONE',  ( 0.000000000000000000, 0.000000000000000000, 1.000000000000000000 ) ) ;
#6808 = CARTESIAN_POINT ( 'NONE',  ( -13.82508104294698015, -29.04416526290806289, 38.16992750791695954 ) ) ;
#6809 = CARTESIAN_POINT ( 'NONE',  ( 1.035533905932738197, 66.50000000000000000, 46.65000000218494591 ) ) ;
#6810 = CARTESIAN_POINT ( 'NONE',  ( -12.35725562635140307, -28.24771351637085459, 18.92382249208304401 ) ) ;
#6811 = CARTESIAN_POINT ( 'NONE',  ( 4.592425496802577917E-16, 61.50000000000000000, 49.39999999999999147 ) ) ;
#6812 = CARTESIAN_POINT ( 'NONE',  ( -25.00000000000000711, 0.000000000000000000, -42.50000000000001421 ) ) ;
#6813 = CARTESIAN_POINT ( 'NONE',  ( -41.00000000000000711, 110.0000000000000000, -31.00000000000000000 ) ) ;
#6814 = CARTESIAN_POINT ( 'NONE',  ( -1.461580736456473462, 62.53841926354353120, 45.85000000109246798 ) ) ;
#6815 = CARTESIAN_POINT ( 'NONE',  ( -10.00000000000000000, 47.00000000000000711, 33.99999999999999289 ) ) ;
#6816 = ORIENTED_EDGE ( 'NONE', *, *, #4645, .T. ) ;
#6817 = SURFACE_SIDE_STYLE ('',( #835 ) ) ;
#6818 = CARTESIAN_POINT ( 'NONE',  ( 0.8561741729129471734, 61.93301270000000613, 45.80000000109246372 ) ) ;
#6819 = CARTESIAN_POINT ( 'NONE',  ( -17.07549068051210739, -21.68318583509881847, 40.35742750791696665 ) ) ;
#6820 = FACE_OUTER_BOUND ( 'NONE', #13893, .T. ) ;
#6821 = CARTESIAN_POINT ( 'NONE',  ( -9.754982604823302594, -29.00369391078756465, 29.20507249208304046 ) ) ;
#6822 = CARTESIAN_POINT ( 'NONE',  ( -2.066987300000001415, 63.14382582708705627, 49.00000000109246656 ) ) ;
#6823 = VERTEX_POINT ( 'NONE', #1877 ) ;
#6824 = CARTESIAN_POINT ( 'NONE',  ( -40.00000000000000000, 53.00000000000000711, 30.00000000000000000 ) ) ;
#6825 = DIRECTION ( 'NONE',  ( 1.156482317317871725E-16, 0.000000000000000000, -1.000000000000000000 ) ) ;
#6826 = CARTESIAN_POINT ( 'NONE',  ( 1.461580736456473906, 62.53841926354353120, 45.85000000109246798 ) ) ;
#6827 = CARTESIAN_POINT ( 'NONE',  ( -24.00000000000000000, 53.00000000000000711, 30.00000000000000000 ) ) ;
#6828 = AXIS2_PLACEMENT_3D ( 'NONE', #5649, #13185, #11611 ) ;
#6829 = CARTESIAN_POINT ( 'NONE',  ( -1.530808498934192803E-16, 66.50000000000000000, 49.79999999999999716 ) ) ;
#6830 = DIRECTION ( 'NONE',  ( 0.000000000000000000, 0.000000000000000000, 1.000000000000000000 ) ) ;
#6831 = CARTESIAN_POINT ( 'NONE',  ( 2.492551403682558675, 27.92836399182260720, 58.20336399182267684 ) ) ;
#6832 = ORIENTED_EDGE ( 'NONE', *, *, #7881, .F. ) ;
#6833 = ORIENTED_EDGE ( 'NONE', *, *, #10449, .T. ) ;
#6834 = CARTESIAN_POINT ( 'NONE',  ( -22.04416526290809486, -22.28918265808477628, 5.142572492083038682 ) ) ;
#6835 = ORIENTED_EDGE ( 'NONE', *, *, #5580, .F. ) ;
#6837 = ORIENTED_EDGE ( 'NONE', *, *, #3184, .F. ) ;
#6836 = ORIENTED_EDGE ( 'NONE', *, *, #6772, .F. ) ;
#6838 = CARTESIAN_POINT ( 'NONE',  ( -14.03132541760400009, -26.95583473709189448, 29.64257249208304401 ) ) ;
#6839 = CARTESIAN_POINT ( 'NONE',  ( -13.28918265808472299, -31.04416526290805933, 27.66992750791695954 ) ) ;
#6840 = VECTOR ( 'NONE', #2207, 1000.000000000000000 ) ;
#6841 = CARTESIAN_POINT ( 'NONE',  ( 5.799999999999984723, 29.74264068711924835, 56.74264068711931230 ) ) ;
#6842 = CARTESIAN_POINT ( 'NONE',  ( 1.035533905932738197, 66.50000000000000000, 48.25000000218493312 ) ) ;
#6843 = DIRECTION ( 'NONE',  ( 0.000000000000000000, 0.000000000000000000, -1.000000000000000000 ) ) ;
#6844 = EDGE_LOOP ( 'NONE', ( #14973, #18165, #12468, #16963 ) ) ;
#6845 = EDGE_CURVE ( 'NONE', #834, #17858, #10966, .T. ) ;
#6846 = CARTESIAN_POINT ( 'NONE',  ( -41.00000000000000711, 110.0000000000000000, 8.000000000000000000 ) ) ;
#6847 = ORIENTED_EDGE ( 'NONE', *, *, #4486, .T. ) ;
#6848 = LINE ( 'NONE', #2532, #9700 ) ;
#6849 = ORIENTED_EDGE ( 'NONE', *, *, #7767, .F. ) ;
#6850 = CARTESIAN_POINT ( 'NONE',  ( -0.1365770217272186116, 61.93313928031658122, 44.99999999999987921 ) ) ;
#6851 = CARTESIAN_POINT ( 'NONE',  ( 0.000000000000000000, 0.000000000000000000, 1.500000000000000000 ) ) ;
#6852 = CARTESIAN_POINT ( 'NONE',  ( -24.00000000000000000, 47.00000000000000711, -67.72004514666936359 ) ) ;
#6853 = AXIS2_PLACEMENT_3D ( 'NONE', #5294, #9791, #9969 ) ;
#6854 = CARTESIAN_POINT ( 'NONE',  ( 2.066987300000002303, 63.14382582708705627, 46.70000000109248361 ) ) ;
#6855 = LINE ( 'NONE', #17733, #947 ) ;
#6856 = AXIS2_PLACEMENT_3D ( 'NONE', #16878, #14124, #2070 ) ;
#6857 = LINE ( 'NONE', #17349, #10813 ) ;
#6858 = DIRECTION ( 'NONE',  ( -0.000000000000000000, 0.7071067811865456854, 0.7071067811865493491 ) ) ;
#6859 = ORIENTED_EDGE ( 'NONE', *, *, #15468, .F. ) ;
#6860 = ORIENTED_EDGE ( 'NONE', *, *, #975, .T. ) ;
#6861 = CARTESIAN_POINT ( 'NONE',  ( -12.35725562635143682, -19.75228648362908501, 36.20117750791695954 ) ) ;
#6862 = CARTESIAN_POINT ( 'NONE',  ( -24.00000000000000000, 110.0000000000000000, -25.49999999999999645 ) ) ;
#6863 = EDGE_CURVE ( 'NONE', #7196, #17051, #16581, .T. ) ;
#6864 = VERTEX_POINT ( 'NONE', #18259 ) ;
#6865 = EDGE_CURVE ( 'NONE', #5230, #17811, #13535, .T. ) ;
#6866 = CARTESIAN_POINT ( 'NONE',  ( -11.46040770435014977, -20.21908421996103655, 27.89257249208303335 ) ) ;
#6867 = EDGE_CURVE ( 'NONE', #17639, #3710, #307, .T. ) ;
#6868 = AXIS2_PLACEMENT_3D ( 'NONE', #14837, #131, #1511 ) ;
#6869 = DIRECTION ( 'NONE',  ( 0.000000000000000000, -1.000000000000000000, 1.320393690296331133E-15 ) ) ;
#6870 = ORIENTED_EDGE ( 'NONE', *, *, #17901, .T. ) ;
#6871 = CARTESIAN_POINT ( 'NONE',  ( -12.31951028609536536, -25.35725562635139596, 28.98632249208304401 ) ) ;
#6872 = AXIS2_PLACEMENT_3D ( 'NONE', #7583, #12079, #1313 ) ;
#6873 = CARTESIAN_POINT ( 'NONE',  ( -2.500000000000001776, 64.00000000000000000, 49.19999999999999574 ) ) ;
#6874 = ORIENTED_EDGE ( 'NONE', *, *, #15356, .T. ) ;
#6875 = LINE ( 'NONE', #11465, #11541 ) ;
#6876 = ORIENTED_EDGE ( 'NONE', *, *, #3646, .T. ) ;
#6877 = CARTESIAN_POINT ( 'NONE',  ( -15.00000000000000000, -37.50000000000000000, -3.000000000000000000 ) ) ;
#6878 = CARTESIAN_POINT ( 'NONE',  ( 0.1249999999999895917, 33.66708332270461312, 52.46464466094069934 ) ) ;
#6879 = LINE ( 'NONE', #5419, #9111 ) ;
#6880 = TOROIDAL_SURFACE ( 'NONE', #19096, 4.000000000000000000, 0.2500000000000000000 ) ;
#6881 = CARTESIAN_POINT ( 'NONE',  ( -9.999999999999994671, -24.16482700510257686, 31.82617750791696309 ) ) ;
#6882 = VECTOR ( 'NONE', #19351, 1000.000000000000000 ) ;
#6883 = FACE_BOUND ( 'NONE', #3127, .T. ) ;
#6884 = DIRECTION ( 'NONE',  ( 0.000000000000000000, 0.000000000000000000, -1.000000000000000000 ) ) ;
#6885 = DIRECTION ( 'NONE',  ( 0.000000000000000000, 0.000000000000000000, -1.000000000000000000 ) ) ;
#6886 = VECTOR ( 'NONE', #12917, 1000.000000000000000 ) ;
#6887 = DIRECTION ( 'NONE',  ( -2.602085213965211135E-16, 1.000000000000000000, -0.000000000000000000 ) ) ;
#6888 = ADVANCED_FACE ( 'NONE', ( #15212, #12263, #1782, #1683, #3352, #9317 ), #7959, .T. ) ;
#6889 = ORIENTED_EDGE ( 'NONE', *, *, #8671, .F. ) ;
#6890 = EDGE_LOOP ( 'NONE', ( #8389, #12934, #16895, #17374 ) ) ;
#6891 = CARTESIAN_POINT ( 'NONE',  ( -10.04416526290807710, -25.50457296725819489, 32.04492750791695954 ) ) ;
#6892 = AXIS2_PLACEMENT_3D ( 'NONE', #2131, #8371, #11680 ) ;
#6893 = CARTESIAN_POINT ( 'NONE',  ( 0.8561741729129460632, 66.06698729999999387, 48.50000000109246656 ) ) ;
#6894 = CARTESIAN_POINT ( 'NONE',  ( -9.999999999999994671, -23.83517299489734143, 28.54882249208304401 ) ) ;
#6895 = DIRECTION ( 'NONE',  ( 0.000000000000000000, -1.000000000000000000, 0.000000000000000000 ) ) ;
#6896 = AXIS2_PLACEMENT_3D ( 'NONE', #10488, #2852, #11856 ) ;
#6897 = CARTESIAN_POINT ( 'NONE',  ( 2.500000000000000000, 0.000000000000000000, 0.000000000000000000 ) ) ;
#6898 = CARTESIAN_POINT ( 'NONE',  ( -12.64274437364855252, -28.41254052147347053, 32.70117750791696665 ) ) ;
#6899 = CARTESIAN_POINT ( 'NONE',  ( 7.500000000000005329, -26.00000000000000000, 1.500000000000000000 ) ) ;
#6900 = CARTESIAN_POINT ( 'NONE',  ( -10.04416526290807710, -25.50457296725819489, 26.79492750791695954 ) ) ;
#6901 = CIRCLE ( 'NONE', #17868, 5.800000000000007816 ) ;
#6902 = DIRECTION ( 'NONE',  ( 0.000000000000000000, -1.224646799147353207E-16, 1.000000000000000000 ) ) ;
#6903 = LINE ( 'NONE', #12875, #6300 ) ;
#6904 = CARTESIAN_POINT ( 'NONE',  ( -1.265664690411616068E-16, 66.06698730000000808, 45.55000000109246372 ) ) ;
#6905 = CARTESIAN_POINT ( 'NONE',  ( -45.00000000000000000, 3.000000000000000000, 54.99999999999998579 ) ) ;
#6906 = PRODUCT_DEFINITION_SHAPE ( 'NONE', 'NONE',  #19412 ) ;
#6907 = ADVANCED_FACE ( 'NONE', ( #15408 ), #6391, .F. ) ;
#6908 = LINE ( 'NONE', #8568, #4286 ) ;
#6909 = CARTESIAN_POINT ( 'NONE',  ( 4.592425496802577917E-16, 61.50000000000000000, 49.39999999999999147 ) ) ;
#6910 = LINE ( 'NONE', #15744, #12689 ) ;
#6911 = ORIENTED_EDGE ( 'NONE', *, *, #14804, .T. ) ;
#6912 = AXIS2_PLACEMENT_3D ( 'NONE', #11712, #3204, #5948 ) ;
#6913 = CARTESIAN_POINT ( 'NONE',  ( 0.000000000000000000, 64.00000000000000000, 34.99999999999999289 ) ) ;
#6914 = CARTESIAN_POINT ( 'NONE',  ( -10.04416526290807710, -25.50457296725819489, 5.794927507916955989 ) ) ;
#6915 = EDGE_CURVE ( 'NONE', #6744, #3230, #18351, .T. ) ;
#6916 = CARTESIAN_POINT ( 'NONE',  ( 1.035533905932738197, 66.50000000000000000, 48.94999999999999574 ) ) ;
#6917 = CARTESIAN_POINT ( 'NONE',  ( -21.14459132904239169, -20.64274437364858628, 26.36132249208303691 ) ) ;
#6918 = CIRCLE ( 'NONE', #1927, 2.999999999999999112 ) ;
#6919 = CARTESIAN_POINT ( 'NONE',  ( 3.796994071234847710E-16, 61.93301269999999903, 49.15000000109246514 ) ) ;
#6920 = ORIENTED_EDGE ( 'NONE', *, *, #659, .T. ) ;
#6921 = CYLINDRICAL_SURFACE ( 'NONE', #10953, 1.500000000000000222 ) ;
#6922 = DIRECTION ( 'NONE',  ( 0.000000000000000000, 0.000000000000000000, -1.000000000000000000 ) ) ;
#6923 = VECTOR ( 'NONE', #17959, 1000.000000000000114 ) ;
#6924 = CARTESIAN_POINT ( 'NONE',  ( 1.461580736456473684, 65.46158073645646880, 46.85000000109246798 ) ) ;
#6925 = DIRECTION ( 'NONE',  ( -7.304098846218135653E-17, 0.000000000000000000, 1.000000000000000000 ) ) ;
#6926 = VECTOR ( 'NONE', #8419, 1000.000000000000000 ) ;
#6927 = CARTESIAN_POINT ( 'NONE',  ( 2.500000000000007550, 65.03553390593272354, 48.95000000218495018 ) ) ;
#6928 = EDGE_CURVE ( 'NONE', #2358, #7475, #12059, .T. ) ;
#6929 = DIRECTION ( 'NONE',  ( 1.000000000000000000, 0.000000000000000000, 0.000000000000000000 ) ) ;
#6930 = CARTESIAN_POINT ( 'NONE',  ( 2.500000000000001776, 64.00000000000000000, 47.99999999999999289 ) ) ;
#6931 = ORIENTED_EDGE ( 'NONE', *, *, #2994, .F. ) ;
#6932 = ORIENTED_EDGE ( 'NONE', *, *, #15362, .T. ) ;
#6933 = CARTESIAN_POINT ( 'NONE',  ( -21.99999999999999289, -24.16482700510262305, 10.17382249208303868 ) ) ;
#6934 = AXIS2_PLACEMENT_3D ( 'NONE', #18896, #11330, #17233 ) ;
#6935 = ORIENTED_EDGE ( 'NONE', *, *, #13803, .T. ) ;
#6937 = ORIENTED_EDGE ( 'NONE', *, *, #17065, .F. ) ;
#6936 = VERTEX_POINT ( 'NONE', #6200 ) ;
#6938 = CARTESIAN_POINT ( 'NONE',  ( -14.36097942780923731, -27.04416526290806999, 6.669927507916960430 ) ) ;
#6939 = CARTESIAN_POINT ( 'NONE',  ( -8.044165262908075320, -26.04047135212042718, 32.04492750791695954 ) ) ;
#6940 = VECTOR ( 'NONE', #8238, 1000.000000000000000 ) ;
#6941 = CARTESIAN_POINT ( 'NONE',  ( 0.000000000000000000, 0.000000000000000000, 1.500000000000000000 ) ) ;
#6942 = CARTESIAN_POINT ( 'NONE',  ( 1.767766952966369987, 65.76776695296638309, 49.00000000218494023 ) ) ;
#6943 = DIRECTION ( 'NONE',  ( 0.000000000000000000, 1.000000000000000000, 0.000000000000000000 ) ) ;
#6944 = ORIENTED_EDGE ( 'NONE', *, *, #6730, .F. ) ;
#6945 = LINE ( 'NONE', #16058, #4749 ) ;
#6946 = VERTEX_POINT ( 'NONE', #13626 ) ;
#6947 = DIRECTION ( 'NONE',  ( 0.000000000000000000, -1.000000000000000000, -0.000000000000000000 ) ) ;
#6948 = VERTEX_POINT ( 'NONE', #4731 ) ;
#6949 = LINE ( 'NONE', #11351, #4125 ) ;
#6950 = CARTESIAN_POINT ( 'NONE',  ( -1.040834085586084257E-14, 27.62132034355962773, 54.62132034355965260 ) ) ;
#6951 = DIRECTION ( 'NONE',  ( 1.000000000000000000, 0.000000000000000000, -4.081702296416016490E-16 ) ) ;
#6952 = CARTESIAN_POINT ( 'NONE',  ( -1.461580736456473906, 65.46158073645646880, 46.25000000109247367 ) ) ;
#6953 = CARTESIAN_POINT ( 'NONE',  ( -1.040834085586084257E-14, 23.37867965644034030, 50.37867965644033319 ) ) ;
#6954 = CARTESIAN_POINT ( 'NONE',  ( 2.500000000000011102, 62.96446609406727646, 49.54999999999999716 ) ) ;
#6955 = CYLINDRICAL_SURFACE ( 'NONE', #7375, 1.249999999999999334 ) ;
#6956 = VERTEX_POINT ( 'NONE', #10687 ) ;
#6957 = ORIENTED_EDGE ( 'NONE', *, *, #3381, .T. ) ;
#6958 = EDGE_CURVE ( 'NONE', #6663, #14186, #15000, .T. ) ;
#6960 = EDGE_CURVE ( 'NONE', #5689, #14223, #15075, .T. ) ;
#6959 = CARTESIAN_POINT ( 'NONE',  ( -21.95583473709191580, -21.95952864787954084, 8.419927507916955989 ) ) ;
#6961 = DIRECTION ( 'NONE',  ( 0.000000000000000000, 0.000000000000000000, -1.000000000000000000 ) ) ;
#6962 = ORIENTED_EDGE ( 'NONE', *, *, #7698, .T. ) ;
#6963 = CARTESIAN_POINT ( 'NONE',  ( -16.64274437364858272, -21.48433729119797420, 5.798822492083043123 ) ) ;
#6964 = EDGE_CURVE ( 'NONE', #3115, #11249, #2910, .T. ) ;
#6965 = CARTESIAN_POINT ( 'NONE',  ( -5.800448907431086987, 29.68308948419218041, 56.80092238452520803 ) ) ;
#6966 = EDGE_LOOP ( 'NONE', ( #9123, #2182, #2046, #13132 ) ) ;
#6967 = CARTESIAN_POINT ( 'NONE',  ( -17.68048971390462754, -22.64274437364856496, 36.86132249208304046 ) ) ;
#6968 = EDGE_CURVE ( 'NONE', #14875, #16369, #19287, .T. ) ;
#6969 = DIRECTION ( 'NONE',  ( 0.000000000000000000, 0.000000000000000000, -1.000000000000000000 ) ) ;
#6970 = ORIENTED_EDGE ( 'NONE', *, *, #15473, .F. ) ;
#6971 = CARTESIAN_POINT ( 'NONE',  ( -1.767766952966370209, 65.76776695296638309, 46.80000000218494449 ) ) ;
#6972 = ORIENTED_EDGE ( 'NONE', *, *, #8125, .T. ) ;
#6973 = FACE_OUTER_BOUND ( 'NONE', #18226, .T. ) ;
#6974 = LINE ( 'NONE', #3939, #5488 ) ;
#6975 = DIRECTION ( 'NONE',  ( -1.000000000000000000, -0.000000000000000000, -0.000000000000000000 ) ) ;
#6976 = ADVANCED_FACE ( 'NONE', ( #1348 ), #16237, .T. ) ;
#6977 =( BOUNDED_CURVE ( )  B_SPLINE_CURVE ( 2, ( #9097, #470, #18423, #12129, #7734, #3515, #1660, #2037, #16750 ),
 .UNSPECIFIED., .F., .F. ) 
 B_SPLINE_CURVE_WITH_KNOTS ( ( 3, 2, 2, 2, 3 ),
 ( 0.5714285714285711748, 0.5892857142857141906, 0.6071428571428569843, 0.6250000000000000000, 0.6428571428571429047 ),
 .UNSPECIFIED. ) 
 CURVE ( )  GEOMETRIC_REPRESENTATION_ITEM ( )  RATIONAL_B_SPLINE_CURVE ( ( 1.000000000000000888, 0.9238795325112857393, 1.000000000000000000, 0.9238795325112867385, 1.000000000000000000, 0.9238795325112867385, 1.000000000000000000, 0.9238795325112867385, 1.000000000000000000 ) ) 
 REPRESENTATION_ITEM ( '' )  );
#6978 = CARTESIAN_POINT ( 'NONE',  ( -10.75228648362910100, -26.64274437364854009, 21.76367750791695599 ) ) ;
#6979 = DIRECTION ( 'NONE',  ( 0.000000000000000000, 0.6139406135149196864, -0.7893522173763268812 ) ) ;
#6980 = FILL_AREA_STYLE_COLOUR ( '', #18541 ) ;
#6981 = DIRECTION ( 'NONE',  ( 0.000000000000000000, 0.000000000000000000, -1.000000000000000000 ) ) ;
#6982 = CARTESIAN_POINT ( 'NONE',  ( -2.283493650000001818, 64.00000000000000000, 49.87500000054622973 ) ) ;
#6983 = ORIENTED_EDGE ( 'NONE', *, *, #19379, .T. ) ;
#6984 = EDGE_CURVE ( 'NONE', #13613, #3035, #5651, .T. ) ;
#6985 = CARTESIAN_POINT ( 'NONE',  ( -11.64274437364859693, -17.85540867095757989, 32.92382249208303335 ) ) ;
#6986 = CARTESIAN_POINT ( 'NONE',  ( -11.21908421996108629, -20.46040770435011069, 31.16992750791695599 ) ) ;
#6987 = CARTESIAN_POINT ( 'NONE',  ( -1.461580736456473906, 65.46158073645646880, 48.65000000109247225 ) ) ;
#6988 = CARTESIAN_POINT ( 'NONE',  ( -12.64274437364858628, -19.58745947852646552, 27.67382249208304046 ) ) ;
#6989 = DIRECTION ( 'NONE',  ( -1.000000000000000000, -0.000000000000000000, -0.000000000000000000 ) ) ;
#6990 = ORIENTED_EDGE ( 'NONE', *, *, #8897, .F. ) ;
#6991 = CARTESIAN_POINT ( 'NONE',  ( 37.50000000000000711, 0.000000000000000000, -47.50000000000000000 ) ) ;
#6992 = CARTESIAN_POINT ( 'NONE',  ( -14.83517299489739649, -18.99999999999997868, 30.51367750791695954 ) ) ;
#6993 = DIRECTION ( 'NONE',  ( 1.000000000000000000, 0.000000000000000000, 0.000000000000000000 ) ) ;
#6994 = FACE_OUTER_BOUND ( 'NONE', #10550, .T. ) ;
#6995 = DIRECTION ( 'NONE',  ( -2.220446049250312588E-16, 0.7071067811865453523, 0.7071067811865496822 ) ) ;
#6996 = LINE ( 'NONE', #920, #15048 ) ;
#6997 = EDGE_CURVE ( 'NONE', #9604, #14297, #16439, .T. ) ;
#6998 = ADVANCED_FACE ( 'NONE', ( #1545 ), #18014, .F. ) ;
#6999 = CARTESIAN_POINT ( 'NONE',  ( -1.530808498934192803E-16, 66.50000000000000000, 49.79999999999999716 ) ) ;
#7000 = CARTESIAN_POINT ( 'NONE',  ( -41.00000000000000000, 52.00000000000000711, -50.00000000000000000 ) ) ;
#7001 = ADVANCED_FACE ( 'NONE', ( #13493 ), #1649, .T. ) ;
#7002 = CARTESIAN_POINT ( 'NONE',  ( -0.8561741729129465073, 61.93301270000000613, 45.10000000109246798 ) ) ;
#7003 = CARTESIAN_POINT ( 'NONE',  ( 14.99999999999998579, 3.000000000000000000, 23.99999999999997158 ) ) ;
#7004 = ORIENTED_EDGE ( 'NONE', *, *, #165, .F. ) ;
#7005 =( NAMED_UNIT ( * ) SI_UNIT ( $, .STERADIAN. ) SOLID_ANGLE_UNIT ( ) );
#7006 = CARTESIAN_POINT ( 'NONE',  ( -1.461580736456473462, 62.53841926354353120, 44.85000000109246798 ) ) ;
#7007 = VECTOR ( 'NONE', #11191, 1000.000000000000000 ) ;
#7008 = CARTESIAN_POINT ( 'NONE',  ( -10.58745947852649927, -21.64274437364853654, -0.1113224920830418047 ) ) ;
#7009 = FACE_OUTER_BOUND ( 'NONE', #12217, .T. ) ;
#7010 = CARTESIAN_POINT ( 'NONE',  ( -11.64274437364859693, -17.85540867095757989, 32.92382249208303335 ) ) ;
#7011 = CARTESIAN_POINT ( 'NONE',  ( 1.461580736456473906, 62.53841926354353120, 48.45000000109246940 ) ) ;
#7012 = ADVANCED_FACE ( 'NONE', ( #75 ), #16146, .T. ) ;
#7013 = LINE ( 'NONE', #9668, #16917 ) ;
#7014 = CARTESIAN_POINT ( 'NONE',  ( 3.399999999999996803, 29.47747564417430155, 56.65425233947098604 ) ) ;
#7015 = CARTESIAN_POINT ( 'NONE',  ( -2.066987300000000971, 63.14382582708704916, 46.40000000109247225 ) ) ;
#7016 = PLANE ( 'NONE',  #14660 ) ;
#7017 = PRESENTATION_LAYER_ASSIGNMENT (  '', '', ( #10457 ) ) ;
#7018 = CARTESIAN_POINT ( 'NONE',  ( 2.500000000000001776, 64.00000000000000000, 48.90000000218494591 ) ) ;
#7019 = AXIS2_PLACEMENT_3D ( 'NONE', #12100, #13670, #1722 ) ;
#7020 = LINE ( 'NONE', #5271, #9115 ) ;
#7021 = DIRECTION ( 'NONE',  ( 0.000000000000000000, 0.000000000000000000, 1.000000000000000000 ) ) ;
#7022 = ORIENTED_EDGE ( 'NONE', *, *, #11228, .T. ) ;
#7023 = ORIENTED_EDGE ( 'NONE', *, *, #10575, .F. ) ;
#7024 = CARTESIAN_POINT ( 'NONE',  ( -8.044165262908093084, -21.95952864787946979, 7.330072492083040459 ) ) ;
#7025 =( NAMED_UNIT ( * ) PLANE_ANGLE_UNIT ( ) SI_UNIT ( $, .RADIAN. ) );
#7026 = ORIENTED_EDGE ( 'NONE', *, *, #17643, .T. ) ;
#7028 = ORIENTED_EDGE ( 'NONE', *, *, #15149, .F. ) ;
#7027 = VERTEX_POINT ( 'NONE', #11625 ) ;
#7029 = CARTESIAN_POINT ( 'NONE',  ( -17.31681416490117087, -21.92450931948788551, 42.33007249208304756 ) ) ;
#7030 = CARTESIAN_POINT ( 'NONE',  ( -7.955834737091916686, -22.28918265808470522, 26.35742750791695954 ) ) ;
#7031 = AXIS2_PLACEMENT_3D ( 'NONE', #13562, #13467, #13864 ) ;
#7032 = AXIS2_PLACEMENT_3D ( 'NONE', #6295, #4830, #16781 ) ;
#7033 = CARTESIAN_POINT ( 'NONE',  ( -25.00000000000000711, -6.000000000000000000, -42.50000000000001421 ) ) ;
#7034 = CARTESIAN_POINT ( 'NONE',  ( 2.500000000000001776, 64.00000000000000000, 46.50000000218494733 ) ) ;
#7035 = DIRECTION ( 'NONE',  ( -0.000000000000000000, 0.8660254037844391517, 0.4999999999999991118 ) ) ;
#7036 = ORIENTED_EDGE ( 'NONE', *, *, #16592, .F. ) ;
#7037 = LINE ( 'NONE', #4502, #15694 ) ;
#7038 = ORIENTED_EDGE ( 'NONE', *, *, #10033, .T. ) ;
#7039 = CARTESIAN_POINT ( 'NONE',  ( -24.00000000000000000, 110.0000000000000000, 6.999999999999999112 ) ) ;
#7040 = ORIENTED_EDGE ( 'NONE', *, *, #18302, .F. ) ;
#7041 = DIRECTION ( 'NONE',  ( 0.000000000000000000, 0.000000000000000000, 1.000000000000000000 ) ) ;
#7042 = DIRECTION ( 'NONE',  ( 1.000000000000000000, 0.000000000000000000, 0.000000000000000000 ) ) ;
#7043 = CARTESIAN_POINT ( 'NONE',  ( -32.50000000000000000, 52.00000000000000711, -35.00000000000000000 ) ) ;
#7044 = CARTESIAN_POINT ( 'NONE',  ( -1.461580736456473462, 62.53841926354353120, 44.85000000109246798 ) ) ;
#7045 = LINE ( 'NONE', #18826, #13144 ) ;
#7046 = AXIS2_PLACEMENT_3D ( 'NONE', #6103, #12067, #11671 ) ;
#7047 = CARTESIAN_POINT ( 'NONE',  ( 2.500000000000001776, 64.00000000000000000, 47.30000000218494449 ) ) ;
#7048 = AXIS2_PLACEMENT_3D ( 'NONE', #5798, #13428, #13 ) ;
#7049 = CARTESIAN_POINT ( 'NONE',  ( 0.1499999999999973577, 0.000000000000000000, 0.000000000000000000 ) ) ;
#7050 = VERTEX_POINT ( 'NONE', #16346 ) ;
#7052 = ORIENTED_EDGE ( 'NONE', *, *, #9001, .F. ) ;
#7051 = ORIENTED_EDGE ( 'NONE', *, *, #189, .T. ) ;
#7053 = CARTESIAN_POINT ( 'NONE',  ( -8.855408670957631401, -20.64274437364852943, -0.1113224920830435533 ) ) ;
#7054 = LINE ( 'NONE', #2361, #16819 ) ;
#7055 = ORIENTED_EDGE ( 'NONE', *, *, #6720, .F. ) ;
#7056 = CARTESIAN_POINT ( 'NONE',  ( -17.95583473709190869, -24.96867458239598037, 9.955072492083044011 ) ) ;
#7057 = CARTESIAN_POINT ( 'NONE',  ( -1.767766952966369765, 62.23223304703363112, 45.29999999999999005 ) ) ;
#7058 = APPLICATION_CONTEXT ( 'automotive_design' ) ;
#7059 = VERTEX_POINT ( 'NONE', #17920 ) ;
#7060 = CARTESIAN_POINT ( 'NONE',  ( -14.83517299489738761, -20.99999999999997513, 9.513677507916957765 ) ) ;
#7061 = VECTOR ( 'NONE', #675, 1000.000000000000000 ) ;
#7062 = SURFACE_STYLE_USAGE ( .BOTH. , #2646 ) ;
#7063 = ORIENTED_EDGE ( 'NONE', *, *, #16757, .F. ) ;
#7064 = VECTOR ( 'NONE', #6150, 1000.000000000000000 ) ;
#7065 = LINE ( 'NONE', #10090, #16907 ) ;
#7066 = EDGE_LOOP ( 'NONE', ( #2807, #5136, #5876, #16194 ) ) ;
#7067 = CARTESIAN_POINT ( 'NONE',  ( -47.00000000000002132, 118.0000000000000142, -60.00000000000002132 ) ) ;
#7068 = EDGE_CURVE ( 'NONE', #15887, #18550, #18281, .T. ) ;
#7069 = LINE ( 'NONE', #6878, #7680 ) ;
#7070 = CARTESIAN_POINT ( 'NONE',  ( -0.9999999999999945599, -28.00000000000000000, 9.500000000000001776 ) ) ;
#7071 = CARTESIAN_POINT ( 'NONE',  ( -1.035533905932738641, 66.50000000000000000, 48.35000000218494165 ) ) ;
#7072 = EDGE_CURVE ( 'NONE', #8851, #8886, #6996, .T. ) ;
#7073 = CARTESIAN_POINT ( 'NONE',  ( -9.955834737091912245, -22.82508104294696594, 26.35742750791695954 ) ) ;
#7074 = DIRECTION ( 'NONE',  ( -1.156482317317871725E-16, 1.000000000000000000, 0.000000000000000000 ) ) ;
#7076 = EDGE_CURVE ( 'NONE', #15771, #13286, #11789, .T. ) ;
#7075 = DIRECTION ( 'NONE',  ( 0.000000000000000000, 0.000000000000000000, 1.000000000000000000 ) ) ;
#7077 = AXIS2_PLACEMENT_3D ( 'NONE', #2862, #8841, #19339 ) ;
#7078 = CARTESIAN_POINT ( 'NONE',  ( -41.00000000000000711, 53.00000000000000711, 8.000000000000000000 ) ) ;
#7079 = ORIENTED_EDGE ( 'NONE', *, *, #10487, .T. ) ;
#7080 = VECTOR ( 'NONE', #14846, 1000.000000000000000 ) ;
#7081 = CARTESIAN_POINT ( 'NONE',  ( -16.17491895705296656, -29.04416526290807710, 9.080072492083036906 ) ) ;
#7082 = CARTESIAN_POINT ( 'NONE',  ( -9.754982604823348780, -18.99630608921234654, -0.3300724920830435116 ) ) ;
#7083 = CARTESIAN_POINT ( 'NONE',  ( 2.066987300000001415, 64.00000000000000000, 47.55000000109247082 ) ) ;
#7084 = CARTESIAN_POINT ( 'NONE',  ( -15.96867458239599635, -21.04416526290806999, 11.26757249208304579 ) ) ;
#7085 = CARTESIAN_POINT ( 'NONE',  ( -2.500000000000001776, 64.00000000000000000, 48.39999999999999858 ) ) ;
#7086 = ORIENTED_EDGE ( 'NONE', *, *, #16547, .F. ) ;
#7087 = CARTESIAN_POINT ( 'NONE',  ( -40.00000000000000000, 53.00000000000000711, 30.00000000000000000 ) ) ;
#7088 = CARTESIAN_POINT ( 'NONE',  ( -10.58745947852649927, -21.64274437364853654, 31.38867750791696309 ) ) ;
#7089 = EDGE_CURVE ( 'NONE', #16934, #5764, #6903, .T. ) ;
#7090 = CARTESIAN_POINT ( 'NONE',  ( -45.00000000000000000, -1.285879139104706187E-16, 56.59999999999998010 ) ) ;
#7091 = VECTOR ( 'NONE', #16372, 1000.000000000000000 ) ;
#7092 = DIRECTION ( 'NONE',  ( 0.000000000000000000, -1.000000000000000000, 0.000000000000000000 ) ) ;
#7093 = CARTESIAN_POINT ( 'NONE',  ( -41.00000000000000711, 53.00000000000000711, 6.999999999999999112 ) ) ;
#7094 = CARTESIAN_POINT ( 'NONE',  ( -12.35725562635140307, -28.24771351637085459, 34.67382249208304046 ) ) ;
#7095 = VECTOR ( 'NONE', #6298, 1000.000000000000000 ) ;
#7096 = CARTESIAN_POINT ( 'NONE',  ( 1.767766952966370653, 62.23223304703363112, 47.89999999999999858 ) ) ;
#7097 = CARTESIAN_POINT ( 'NONE',  ( 2.066987300000001415, 64.00000000000000000, 49.35000000109246798 ) ) ;
#7098 = DIRECTION ( 'NONE',  ( -0.000000000000000000, -1.000000000000000000, -0.000000000000000000 ) ) ;
#7099 = CARTESIAN_POINT ( 'NONE',  ( 2.500000000000001776, 65.03553390593273775, 48.85000000000000142 ) ) ;
#7100 = DIRECTION ( 'NONE',  ( 0.000000000000000000, 0.000000000000000000, 1.000000000000000000 ) ) ;
#7101 = VERTEX_POINT ( 'NONE', #11395 ) ;
#7102 =( NAMED_UNIT ( * ) PLANE_ANGLE_UNIT ( ) SI_UNIT ( $, .RADIAN. ) );
#7103 = EDGE_CURVE ( 'NONE', #18913, #1793, #12966, .T. ) ;
#7104 = CARTESIAN_POINT ( 'NONE',  ( -13.82508104294698192, -29.04416526290806644, 6.669927507916955989 ) ) ;
#7105 = EDGE_CURVE ( 'NONE', #262, #11814, #2838, .T. ) ;
#7106 = CARTESIAN_POINT ( 'NONE',  ( -16.50457296725820555, -28.95583473709189448, 1.857427507916957765 ) ) ;
#7107 = FACE_BOUND ( 'NONE', #10188, .T. ) ;
#7108 = EDGE_CURVE ( 'NONE', #14101, #14697, #1615, .T. ) ;
#7109 = CARTESIAN_POINT ( 'NONE',  ( -8.855408670957602979, -27.35725562635137820, 28.98632249208304401 ) ) ;
#7110 = CARTESIAN_POINT ( 'NONE',  ( -0.8561741729129461742, 66.06698729999999387, 47.20000000109247651 ) ) ;
#7111 = CARTESIAN_POINT ( 'NONE',  ( -17.51566270880201159, -22.35725562635141728, 34.88867750791696665 ) ) ;
#7112 = CARTESIAN_POINT ( 'NONE',  ( -16.17491895705301275, -18.95583473709189448, 9.294927507916955989 ) ) ;
#7113 = CARTESIAN_POINT ( 'NONE',  ( -14.99999999999999645, 47.00000000000000711, 26.99999999999997868 ) ) ;
#7114 = CARTESIAN_POINT ( 'NONE',  ( -12.50000000000000000, -35.50000000000000000, 1.500000000000000000 ) ) ;
#7115 = FACE_OUTER_BOUND ( 'NONE', #9891, .T. ) ;
#7116 = CARTESIAN_POINT ( 'NONE',  ( -1.461580736456473906, 65.46158073645646880, 49.65000000109246514 ) ) ;
#7117 = DIRECTION ( 'NONE',  ( 1.000000000000000000, 0.000000000000000000, 0.000000000000000000 ) ) ;
#7118 = DIRECTION ( 'NONE',  ( 1.000000000000000000, 0.000000000000000000, 0.000000000000000000 ) ) ;
#7119 = EDGE_CURVE ( 'NONE', #13602, #13902, #9247, .T. ) ;
#7120 = ORIENTED_EDGE ( 'NONE', *, *, #314, .F. ) ;
#7121 = ORIENTED_EDGE ( 'NONE', *, *, #3967, .F. ) ;
#7122 = EDGE_CURVE ( 'NONE', #16368, #6094, #17978, .T. ) ;
#7123 = CARTESIAN_POINT ( 'NONE',  ( -22.04416526290809486, -22.28918265808477628, 10.39257249208303691 ) ) ;
#7124 =( NAMED_UNIT ( * ) PLANE_ANGLE_UNIT ( ) SI_UNIT ( $, .RADIAN. ) );
#7125 = EDGE_LOOP ( 'NONE', ( #9588, #17744, #13529, #3241 ) ) ;
#7127 = ORIENTED_EDGE ( 'NONE', *, *, #14798, .T. ) ;
#7126 = EDGE_LOOP ( 'NONE', ( #5860, #8497, #18225, #15673 ) ) ;
#7128 = CARTESIAN_POINT ( 'NONE',  ( -17.07549068051208963, -26.31681416490115311, 41.01757249208304756 ) ) ;
#7129 = CARTESIAN_POINT ( 'NONE',  ( -17.04047135212043784, -30.95583473709190159, 28.10742750791695954 ) ) ;
#7130 = LINE ( 'NONE', #18906, #2249 ) ;
#7131 = CARTESIAN_POINT ( 'NONE',  ( 1.035533905932738197, 66.50000000000000000, 45.05000000218494449 ) ) ;
#7132 = FACE_OUTER_BOUND ( 'NONE', #1988, .T. ) ;
#7133 = VERTEX_POINT ( 'NONE', #13361 ) ;
#7134 = DIRECTION ( 'NONE',  ( 0.000000000000000000, 1.000000000000000000, 0.000000000000000000 ) ) ;
#7135 = VERTEX_POINT ( 'NONE', #3175 ) ;
#7136 = CARTESIAN_POINT ( 'NONE',  ( -7.999999999999996447, 0.000000000000000000, 0.000000000000000000 ) ) ;
#7137 = VERTEX_POINT ( 'NONE', #7685 ) ;
#7138 = CARTESIAN_POINT ( 'NONE',  ( -15.00000000000000000, -32.00000000000000711, -3.000000000000000000 ) ) ;
#7139 = CARTESIAN_POINT ( 'NONE',  ( -37.50000000000002132, 107.3545527679194436, 24.99999999999998224 ) ) ;
#7140 = LINE ( 'NONE', #13107, #10615 ) ;
#7141 = CARTESIAN_POINT ( 'NONE',  ( 2.066987300000001415, 64.00000000000000000, 46.75000000109247367 ) ) ;
#7142 = DIRECTION ( 'NONE',  ( 0.000000000000000000, -0.000000000000000000, -1.000000000000000000 ) ) ;
#7143 = CARTESIAN_POINT ( 'NONE',  ( -1.035533905932738863, 61.50000000000000000, 49.35000000000000853 ) ) ;
#7144 = LINE ( 'NONE', #8616, #5188 ) ;
#7145 = EDGE_CURVE ( 'NONE', #14590, #10761, #7785, .T. ) ;
#7146 = ORIENTED_EDGE ( 'NONE', *, *, #12750, .F. ) ;
#7148 = VERTEX_POINT ( 'NONE', #18082 ) ;
#7147 = ORIENTED_EDGE ( 'NONE', *, *, #3776, .F. ) ;
#7149 = CARTESIAN_POINT ( 'NONE',  ( -12.95952864787955150, -17.04416526290805933, 4.482427507916956877 ) ) ;
#7150 = VECTOR ( 'NONE', #16026, 1000.000000000000000 ) ;
#7151 = DIRECTION ( 'NONE',  ( -1.000000000000000000, 0.000000000000000000, -1.156482317317871725E-16 ) ) ;
#7152 = ORIENTED_EDGE ( 'NONE', *, *, #9532, .T. ) ;
#7153 = CARTESIAN_POINT ( 'NONE',  ( -19.24771351637086880, -26.64274437364857206, 41.23632249208304046 ) ) ;
#7154 = CARTESIAN_POINT ( 'NONE',  ( -1.035533905932738641, 66.50000000000000000, 45.04999999999999005 ) ) ;
#7155 = ORIENTED_EDGE ( 'NONE', *, *, #1203, .T. ) ;
#7156 = CARTESIAN_POINT ( 'NONE',  ( -15.16482700510262482, -20.99999999999997513, 42.98632249208304756 ) ) ;
#7157 = VECTOR ( 'NONE', #10778, 1000.000000000000000 ) ;
#7158 = CARTESIAN_POINT ( 'NONE',  ( -15.00000000000000000, 0.000000000000000000, 0.000000000000000000 ) ) ;
#7159 = ORIENTED_EDGE ( 'NONE', *, *, #7605, .F. ) ;
#7160 = LINE ( 'NONE', #7455, #12201 ) ;
#7161 = ORIENTED_EDGE ( 'NONE', *, *, #10010, .T. ) ;
#7162 = CARTESIAN_POINT ( 'NONE',  ( -2.500000000000001776, 64.00000000000000000, 47.59999999999999432 ) ) ;
#7163 = DIRECTION ( 'NONE',  ( -1.541976423090495633E-16, 0.000000000000000000, 1.000000000000000000 ) ) ;
#7164 = VECTOR ( 'NONE', #353, 1000.000000000000000 ) ;
#7165 = DIRECTION ( 'NONE',  ( 0.000000000000000000, 0.000000000000000000, 1.000000000000000000 ) ) ;
#7166 = APPLICATION_PROTOCOL_DEFINITION ( 'draft international standard', 'automotive_design', 1998, #19088 ) ;
#7167 = LINE ( 'NONE', #14170, #12267 ) ;
#7168 = CARTESIAN_POINT ( 'NONE',  ( -12.64274437364855252, -28.41254052147347053, 32.70117750791696665 ) ) ;
#7169 = DIRECTION ( 'NONE',  ( -0.000000000000000000, -0.000000000000000000, -1.000000000000000000 ) ) ;
#7170 = CARTESIAN_POINT ( 'NONE',  ( -10.75228648362910100, -26.64274437364854009, 0.7636775079169582092 ) ) ;
#7171 = VECTOR ( 'NONE', #973, 1000.000000000000000 ) ;
#7172 = DIRECTION ( 'NONE',  ( 0.000000000000000000, 1.000000000000000000, 0.000000000000000000 ) ) ;
#7173 = ORIENTED_EDGE ( 'NONE', *, *, #2198, .T. ) ;
#7174 = CARTESIAN_POINT ( 'NONE',  ( -21.95583473709189803, -26.04047135212049469, 41.45507249208303335 ) ) ;
#7175 = VECTOR ( 'NONE', #9529, 1000.000000000000000 ) ;
#7176 = CARTESIAN_POINT ( 'NONE',  ( -11.35725562635144925, -18.02023567606020293, 4.701177507916955989 ) ) ;
#7177 = VECTOR ( 'NONE', #17729, 1000.000000000000000 ) ;
#7178 = CARTESIAN_POINT ( 'NONE',  ( 0.000000000000000000, 64.00000000000000000, 49.99999999999999289 ) ) ;
#7179 = CARTESIAN_POINT ( 'NONE',  ( -20.04416526290809131, -22.82508104294699791, 41.89257249208301914 ) ) ;
#7180 = DIRECTION ( 'NONE',  ( 0.000000000000000000, 0.000000000000000000, 1.000000000000000000 ) ) ;
#7181 = ORIENTED_EDGE ( 'NONE', *, *, #18854, .F. ) ;
#7182 = CARTESIAN_POINT ( 'NONE',  ( -41.00000000000000711, 53.00000000000000711, 26.50000000000000000 ) ) ;
#7183 = DIRECTION ( 'NONE',  ( 0.000000000000000000, 1.000000000000000000, 0.000000000000000000 ) ) ;
#7184 = CARTESIAN_POINT ( 'NONE',  ( 1.753982408753060440, -43.60761626555502346, 1.500000000000000000 ) ) ;
#7186 = LINE ( 'NONE', #12964, #12211 ) ;
#7185 = AXIS2_PLACEMENT_3D ( 'NONE', #4652, #8747, #10805 ) ;
#7187 = FACE_OUTER_BOUND ( 'NONE', #18728, .T. ) ;
#7188 = CARTESIAN_POINT ( 'NONE',  ( -12.64274437364858628, -19.58745947852646552, 32.92382249208304046 ) ) ;
#7189 = CARTESIAN_POINT ( 'NONE',  ( 1.767766952966369987, 65.76776695296638309, 48.09999999999999432 ) ) ;
#7190 = LINE ( 'NONE', #17391, #7150 ) ;
#7191 = AXIS2_PLACEMENT_3D ( 'NONE', #12448, #14017, #3349 ) ;
#7192 = LINE ( 'NONE', #12779, #9523 ) ;
#7193 = CARTESIAN_POINT ( 'NONE',  ( -2.500000000000000888, 62.96446609406726935, 45.24999999999999289 ) ) ;
#7194 = DIRECTION ( 'NONE',  ( 0.000000000000000000, -1.000000000000000000, -0.000000000000000000 ) ) ;
#7195 = AXIS2_PLACEMENT_3D ( 'NONE', #16378, #5888, #8826 ) ;
#7196 = VERTEX_POINT ( 'NONE', #4654 ) ;
#7197 = ADVANCED_FACE ( 'NONE', ( #6027 ), #7589, .F. ) ;
#7198 = EDGE_CURVE ( 'NONE', #209, #17838, #19353, .T. ) ;
#7199 = SURFACE_SIDE_STYLE ('',( #19265 ) ) ;
#7200 = CARTESIAN_POINT ( 'NONE',  ( -10.58745947852649927, -21.64274437364853654, 10.38867750791695777 ) ) ;
#7201 = VECTOR ( 'NONE', #1751, 1000.000000000000000 ) ;
#7202 = CARTESIAN_POINT ( 'NONE',  ( -12.64274437364855252, -28.41254052147347053, 1.201177507916958431 ) ) ;
#7203 = CARTESIAN_POINT ( 'NONE',  ( 3.999999999999998224, 67.00000000000000000, 34.99999999999999289 ) ) ;
#7204 = CARTESIAN_POINT ( 'NONE',  ( -19.99999999999999645, -24.16482700510261949, 4.923822492083040459 ) ) ;
#7205 = AXIS2_PLACEMENT_3D ( 'NONE', #1886, #16988, #7871 ) ;
#7206 = CARTESIAN_POINT ( 'NONE',  ( 2.066987300000001859, 64.85617417291294373, 47.00000000109246656 ) ) ;
#7207 = CARTESIAN_POINT ( 'NONE',  ( -11.99999999999999289, -24.16482700510258752, 37.07617750791695954 ) ) ;
#7208 = CARTESIAN_POINT ( 'NONE',  ( -18.78091578003889595, -27.53959229564985023, 2.294927507916958209 ) ) ;
#7209 = CARTESIAN_POINT ( 'NONE',  ( 32.50000000000000000, -6.000000000000000000, -45.00000000000000000 ) ) ;
#7210 = VECTOR ( 'NONE', #8076, 1000.000000000000000 ) ;
#7211 = DIRECTION ( 'NONE',  ( -0.000000000000000000, -1.000000000000000000, -0.000000000000000000 ) ) ;
#7212 = DIRECTION ( 'NONE',  ( 0.5773502691896335026, 0.8164965809277204833, 0.000000000000000000 ) ) ;
#7213 = FACE_OUTER_BOUND ( 'NONE', #12120, .T. ) ;
#7214 = VECTOR ( 'NONE', #13556, 1000.000000000000000 ) ;
#7215 = ADVANCED_FACE ( 'NONE', ( #7482, #18282 ), #5919, .T. ) ;
#7216 = CARTESIAN_POINT ( 'NONE',  ( -0.8561741729129461742, 66.06698730000000808, 48.00000000109246656 ) ) ;
#7217 = PLANE ( 'NONE',  #967 ) ;
#7218 = EDGE_CURVE ( 'NONE', #8108, #13491, #10340, .T. ) ;
#7219 = VECTOR ( 'NONE', #759, 1000.000000000000000 ) ;
#7220 = CARTESIAN_POINT ( 'NONE',  ( -1.767766952966369765, 62.23223304703363112, 44.60000000218494165 ) ) ;
#7221 = ORIENTED_EDGE ( 'NONE', *, *, #15617, .T. ) ;
#7222 = ORIENTED_EDGE ( 'NONE', *, *, #17739, .T. ) ;
#7223 = CARTESIAN_POINT ( 'NONE',  ( -16.71081734191520596, -31.04416526290808065, 9.080072492083038682 ) ) ;
#7224 =( NAMED_UNIT ( * ) SI_UNIT ( $, .STERADIAN. ) SOLID_ANGLE_UNIT ( ) );
#7225 = AXIS2_PLACEMENT_3D ( 'NONE', #1382, #10582, #8920 ) ;
#7226 = CARTESIAN_POINT ( 'NONE',  ( -35.00000000000002132, -6.000000000000000000, -42.50000000000001421 ) ) ;
#7228 = EDGE_LOOP ( 'NONE', ( #10844, #419, #8313, #5817 ) ) ;
#7227 = EDGE_LOOP ( 'NONE', ( #11438, #5382, #10988, #12802 ) ) ;
#7229 = CARTESIAN_POINT ( 'NONE',  ( -14.36097942780923731, -27.04416526290806999, 1.419927507916959986 ) ) ;
#7230 = CARTESIAN_POINT ( 'NONE',  ( -13.28918265808478694, -16.95583473709189093, 11.70507249208304046 ) ) ;
#7231 = VECTOR ( 'NONE', #3940, 1000.000000000000000 ) ;
#7232 = CARTESIAN_POINT ( 'NONE',  ( 2.066987300000002303, 63.14382582708705627, 49.10000000109246088 ) ) ;
#7233 = ORIENTED_EDGE ( 'NONE', *, *, #2492, .T. ) ;
#7234 = VERTEX_POINT ( 'NONE', #16408 ) ;
#7235 = AXIS2_PLACEMENT_3D ( 'NONE', #17286, #6884, #11379 ) ;
#7236 = CARTESIAN_POINT ( 'NONE',  ( -2.315774708385926139, 31.32836399182264842, 54.80336399182263563 ) ) ;
#7237 = ORIENTED_EDGE ( 'NONE', *, *, #5345, .F. ) ;
#7238 = ORIENTED_EDGE ( 'NONE', *, *, #887, .F. ) ;
#7239 = CARTESIAN_POINT ( 'NONE',  ( 34.99999999999999289, -6.000000000000000000, 42.49999999999997868 ) ) ;
#7240 = DIRECTION ( 'NONE',  ( 1.000000000000000000, 0.000000000000000000, 0.000000000000000000 ) ) ;
#7241 = LINE ( 'NONE', #11353, #3748 ) ;
#7242 = AXIS2_PLACEMENT_3D ( 'NONE', #752, #471, #6365 ) ;
#7243 = CARTESIAN_POINT ( 'NONE',  ( 2.066987300000001859, 64.85617417291294373, 48.60000000109246798 ) ) ;
#7244 = EDGE_CURVE ( 'NONE', #6946, #10557, #14111, .T. ) ;
#7245 = ADVANCED_FACE ( 'NONE', ( #2973 ), #9051, .F. ) ;
#7246 = CARTESIAN_POINT ( 'NONE',  ( 0.000000000000000000, -0.7390083445627200209, 1.280000000000001137 ) ) ;
#7247 = VECTOR ( 'NONE', #8204, 1000.000000000000000 ) ;
#7248 = CARTESIAN_POINT ( 'NONE',  ( -2.499999999999996003, 62.96446609406726225, 46.95000000218494307 ) ) ;
#7249 = CARTESIAN_POINT ( 'NONE',  ( -12.50000000000000000, -35.50000000000000000, 5.500000000000000000 ) ) ;
#7250 = ORIENTED_EDGE ( 'NONE', *, *, #18974, .F. ) ;
#7252 = EDGE_LOOP ( 'NONE', ( #4194, #5394, #15586, #4365 ) ) ;
#7251 = ORIENTED_EDGE ( 'NONE', *, *, #7610, .T. ) ;
#7253 = ADVANCED_FACE ( 'NONE', ( #14944 ), #6320, .F. ) ;
#7254 = CARTESIAN_POINT ( 'NONE',  ( -19.24771351637089367, -21.35725562635142438, 40.13867750791695954 ) ) ;
#7255 = CARTESIAN_POINT ( 'NONE',  ( 0.000000000000000000, -6.000000000000000000, 0.000000000000000000 ) ) ;
#7256 = ORIENTED_EDGE ( 'NONE', *, *, #11176, .T. ) ;
#7257 = VERTEX_POINT ( 'NONE', #12183 ) ;
#7258 = CARTESIAN_POINT ( 'NONE',  ( -17.07549068051208963, -26.31681416490115311, 4.267572492083044011 ) ) ;
#7259 = FACE_OUTER_BOUND ( 'NONE', #8218, .T. ) ;
#7260 = VERTEX_POINT ( 'NONE', #18182 ) ;
#7261 = CARTESIAN_POINT ( 'NONE',  ( -12.31951028609537602, -22.64274437364854364, -0.1113224920830400977 ) ) ;
#7262 = CARTESIAN_POINT ( 'NONE',  ( 1.767766952966369987, 65.76776695296638309, 47.40000000218494591 ) ) ;
#7263 = ORIENTED_EDGE ( 'NONE', *, *, #7572, .F. ) ;
#7264 = CARTESIAN_POINT ( 'NONE',  ( 3.399999999999996803, 29.65425233947093631, 56.83102903476762435 ) ) ;
#7265 = ORIENTED_EDGE ( 'NONE', *, *, #14625, .T. ) ;
#7266 = ADVANCED_FACE ( 'NONE', ( #1515 ), #14841, .F. ) ;
#7267 = DIRECTION ( 'NONE',  ( 0.000000000000000000, 0.000000000000000000, -1.000000000000000000 ) ) ;
#7268 = PLANE ( 'NONE',  #18651 ) ;
#7269 = SHAPE_REPRESENTATION ( 'spring', ( #1791 ), #2725 ) ;
#7270 = AXIS2_PLACEMENT_3D ( 'NONE', #13868, #14061, #539 ) ;
#7271 = DIRECTION ( 'NONE',  ( 0.000000000000000000, 0.000000000000000000, 1.000000000000000000 ) ) ;
#7272 = SHAPE_DEFINITION_REPRESENTATION ( #1289, #6533 ) ;
#7273 = DIRECTION ( 'NONE',  ( 0.000000000000000000, -1.000000000000000000, 0.000000000000000000 ) ) ;
#7274 = CARTESIAN_POINT ( 'NONE',  ( -19.24771351637089367, -21.35725562635142438, 29.63867750791695599 ) ) ;
#7275 = DIRECTION ( 'NONE',  ( -0.000000000000000000, -1.000000000000000000, -0.000000000000000000 ) ) ;
#7276 = CARTESIAN_POINT ( 'NONE',  ( -19.24771351637089367, -21.35725562635142438, 8.638677507916957765 ) ) ;
#7277 = DIRECTION ( 'NONE',  ( 0.000000000000000000, 1.000000000000000000, -0.000000000000000000 ) ) ;
#7278 = ORIENTED_EDGE ( 'NONE', *, *, #10580, .T. ) ;
#7279 = CARTESIAN_POINT ( 'NONE',  ( -16.17491895705296656, -29.04416526290807710, 3.830072492083041347 ) ) ;
#7280 = CARTESIAN_POINT ( 'NONE',  ( -9.020235676060220698, -27.64274437364852588, 0.7636775079169565439 ) ) ;
#7281 = CARTESIAN_POINT ( 'NONE',  ( -0.8561741729129461742, 66.06698729999999387, 45.40000000109246514 ) ) ;
#7282 = CARTESIAN_POINT ( 'NONE',  ( -14.36097942780925685, -20.95583473709189093, 6.455072492083044899 ) ) ;
#7283 = CARTESIAN_POINT ( 'NONE',  ( -25.00000000000000000, 110.0000000000000000, 30.00000000000000000 ) ) ;
#7284 = ORIENTED_EDGE ( 'NONE', *, *, #12644, .F. ) ;
#7285 = CARTESIAN_POINT ( 'NONE',  ( -10.18851321905033913, -22.11378838432466409, 4.586222366145915297E-17 ) ) ;
#7286 = ORIENTED_EDGE ( 'NONE', *, *, #17408, .F. ) ;
#7287 = PLANE ( 'NONE',  #15329 ) ;
#7288 = DIRECTION ( 'NONE',  ( -1.000000000000000000, 0.000000000000000000, 0.000000000000000000 ) ) ;
#7289 = CARTESIAN_POINT ( 'NONE',  ( -16.17491895705301275, -18.95583473709189448, 40.79492750791696665 ) ) ;
#7290 = FACE_BOUND ( 'NONE', #14670, .T. ) ;
#7291 = CARTESIAN_POINT ( 'NONE',  ( -15.16482700510263371, -18.99999999999997868, 32.48632249208304046 ) ) ;
#7292 = CARTESIAN_POINT ( 'NONE',  ( -1.035533905932738641, 66.50000000000000000, 47.44999999999999574 ) ) ;
#7293 = CARTESIAN_POINT ( 'NONE',  ( 3.796994071234847710E-16, 61.93301269999999903, 47.55000000109247082 ) ) ;
#7294 = SURFACE_STYLE_FILL_AREA ( #13558 ) ;
#7295 = CARTESIAN_POINT ( 'NONE',  ( -1.767766952966369765, 62.23223304703363112, 46.89999999999999858 ) ) ;
#7296 = DIRECTION ( 'NONE',  ( -0.000000000000000000, -1.000000000000000000, -0.000000000000000000 ) ) ;
#7297 = EDGE_LOOP ( 'NONE', ( #8169, #13921, #4317, #16234 ) ) ;
#7298 = CARTESIAN_POINT ( 'NONE',  ( -16.50457296725820555, -28.95583473709189448, 1.857427507916957765 ) ) ;
#7299 = CARTESIAN_POINT ( 'NONE',  ( -15.16482700510259640, -28.99999999999998224, 17.38867750791695599 ) ) ;
#7300 = CARTESIAN_POINT ( 'NONE',  ( 1.767766952966370653, 62.23223304703363112, 48.00000000218494023 ) ) ;
#7301 = CARTESIAN_POINT ( 'NONE',  ( -16.71081734191520596, -31.04416526290808065, 40.58007249208304756 ) ) ;
#7302 = CARTESIAN_POINT ( 'NONE',  ( 2.066987300000001859, 64.85617417291294373, 45.40000000109246514 ) ) ;
#7303 = CARTESIAN_POINT ( 'NONE',  ( -12.92450931948788906, -26.31681416490114245, 37.73242750791696665 ) ) ;
#7304 = CARTESIAN_POINT ( 'NONE',  ( -13.49542703274178201, -19.04416526290806289, 9.732427507916957765 ) ) ;
#7305 = LINE ( 'NONE', #16331, #15309 ) ;
#7306 = DIRECTION ( 'NONE',  ( 1.000000000000000000, -0.000000000000000000, -0.000000000000000000 ) ) ;
#7307 = CARTESIAN_POINT ( 'NONE',  ( -2.749999999999989786, 38.00000000000000000, -42.68883962248118991 ) ) ;
#7308 = EDGE_CURVE ( 'NONE', #13355, #18598, #1914, .T. ) ;
#7309 = EDGE_CURVE ( 'NONE', #3066, #7522, #16707, .T. ) ;
#7310 = DIRECTION ( 'NONE',  ( -7.304098846218135653E-17, 0.000000000000000000, 1.000000000000000000 ) ) ;
#7311 = CARTESIAN_POINT ( 'NONE',  ( 2.500000000000000000, 2.357898499370431722, -2.818925648462311528E-15 ) ) ;
#7312 = CARTESIAN_POINT ( 'NONE',  ( 5.799999999999985612, 29.47747564417429444, 56.65425233947099315 ) ) ;
#7313 = ADVANCED_FACE ( 'NONE', ( #3275 ), #17096, .T. ) ;
#7314 = CARTESIAN_POINT ( 'NONE',  ( -1.035533905932738863, 61.50000000000000000, 44.65000000218493881 ) ) ;
#7315 = EDGE_LOOP ( 'NONE', ( #4879, #9012, #11065, #12605 ) ) ;
#7316 = ORIENTED_EDGE ( 'NONE', *, *, #14178, .T. ) ;
#7317 = CARTESIAN_POINT ( 'NONE',  ( -21.14459132904239169, -20.64274437364858628, 21.11132249208304046 ) ) ;
#7318 = EDGE_CURVE ( 'NONE', #12423, #4121, #15526, .T. ) ;
#7319 =( NAMED_UNIT ( * ) PLANE_ANGLE_UNIT ( ) SI_UNIT ( $, .RADIAN. ) );
#7320 = CARTESIAN_POINT ( 'NONE',  ( -1.530808498934192803E-16, 66.50000000000000000, 47.39999999999999858 ) ) ;
#7322 = EDGE_LOOP ( 'NONE', ( #3933, #1455, #18135, #10308, #9181 ) ) ;
#7321 = VERTEX_POINT ( 'NONE', #2096 ) ;
#7323 = CARTESIAN_POINT ( 'NONE',  ( -12.68318583509884157, -21.92450931948787485, 4.919927507916961318 ) ) ;
#7324 = FACE_OUTER_BOUND ( 'NONE', #7556, .T. ) ;
#7325 = CARTESIAN_POINT ( 'NONE',  ( -21.95583473709189803, -26.04047135212049469, 4.705072492083038682 ) ) ;
#7326 = DIRECTION ( 'NONE',  ( -1.000000000000000000, -0.000000000000000000, -0.000000000000000000 ) ) ;
#7327 = CARTESIAN_POINT ( 'NONE',  ( -2.500000000000001776, 64.00000000000000000, 44.50000000218494733 ) ) ;
#7328 = EDGE_LOOP ( 'NONE', ( #5115, #5854, #6457, #3533 ) ) ;
#7329 = ORIENTED_EDGE ( 'NONE', *, *, #18148, .T. ) ;
#7330 = CARTESIAN_POINT ( 'NONE',  ( -41.00000000000000711, 110.0000000000000000, 0.5000000000000004441 ) ) ;
#7331 = VERTEX_POINT ( 'NONE', #18381 ) ;
#7332 = VECTOR ( 'NONE', #15832, 1000.000000000000000 ) ;
#7333 = VERTEX_POINT ( 'NONE', #11005 ) ;
#7334 = LINE ( 'NONE', #7636, #16236 ) ;
#7335 = CARTESIAN_POINT ( 'NONE',  ( -40.00000000000000711, 113.0000000000000000, 30.00000000000000000 ) ) ;
#7336 = CARTESIAN_POINT ( 'NONE',  ( -2.066987300000001415, 64.00000000000000000, 47.35000000109246798 ) ) ;
#7337 = DIRECTION ( 'NONE',  ( 0.000000000000000000, 0.000000000000000000, -1.000000000000000000 ) ) ;
#7338 = DIRECTION ( 'NONE',  ( 1.000000000000000000, 0.000000000000000000, 2.973811673103096679E-16 ) ) ;
#7339 = EDGE_LOOP ( 'NONE', ( #8908, #9480 ) ) ;
#7341 = ORIENTED_EDGE ( 'NONE', *, *, #4508, .F. ) ;
#7340 = VERTEX_POINT ( 'NONE', #18754 ) ;
#7342 = CARTESIAN_POINT ( 'NONE',  ( -14.83517299489740715, -16.99999999999997868, 14.76367750791695777 ) ) ;
#7343 = STYLED_ITEM ( 'NONE', ( #3974 ), #11772 ) ;
#7344 = DIRECTION ( 'NONE',  ( -1.000000000000000000, 0.000000000000000000, -0.000000000000000000 ) ) ;
#7345 = EDGE_LOOP ( 'NONE', ( #19264, #12178, #6859, #14515 ) ) ;
#7346 = AXIS2_PLACEMENT_3D ( 'NONE', #3771, #2112, #3385 ) ;
#7347 = ORIENTED_EDGE ( 'NONE', *, *, #3184, .T. ) ;
#7348 = CARTESIAN_POINT ( 'NONE',  ( -12.48433729119799196, -22.35725562635139596, 7.111322492083044011 ) ) ;
#7349 = EDGE_CURVE ( 'NONE', #16683, #12144, #11099, .T. ) ;
#7350 = EDGE_CURVE ( 'NONE', #13623, #19197, #12581, .T. ) ;
#7351 = CARTESIAN_POINT ( 'NONE',  ( -37.50000000000002132, -6.000000000000000000, 44.99999999999997868 ) ) ;
#7352 = EDGE_LOOP ( 'NONE', ( #18802, #11745, #13851, #16995 ) ) ;
#7353 = EDGE_CURVE ( 'NONE', #6748, #7898, #5142, .T. ) ;
#7354 = CARTESIAN_POINT ( 'NONE',  ( -14.03132541760400009, -26.95583473709189448, 40.14257249208306177 ) ) ;
#7355 = CARTESIAN_POINT ( 'NONE',  ( -44.99999999999998579, 6.000000000000000000, -56.50000000000000000 ) ) ;
#7356 = ORIENTED_EDGE ( 'NONE', *, *, #9841, .F. ) ;
#7357 = LINE ( 'NONE', #7264, #13128 ) ;
#7358 = EDGE_LOOP ( 'NONE', ( #18640, #16800, #4191, #17423 ) ) ;
#7359 = CARTESIAN_POINT ( 'NONE',  ( -41.00000000000000711, 110.0000000000000000, -44.00000000000000000 ) ) ;
#7360 = EDGE_CURVE ( 'NONE', #8784, #7135, #15434, .T. ) ;
#7361 = CARTESIAN_POINT ( 'NONE',  ( -0.9999999999999945599, -28.00000000000000000, 4.500000000000000888 ) ) ;
#7362 = ORIENTED_EDGE ( 'NONE', *, *, #5451, .F. ) ;
#7363 = FACE_OUTER_BOUND ( 'NONE', #1863, .T. ) ;
#7364 = AXIS2_PLACEMENT_3D ( 'NONE', #2461, #14424, #13035 ) ;
#7365 = DIRECTION ( 'NONE',  ( 1.000000000000000000, 0.000000000000000000, 0.000000000000000000 ) ) ;
#7366 = CARTESIAN_POINT ( 'NONE',  ( -40.00000000000000711, 113.0000000000000000, -31.00000000000000000 ) ) ;
#7367 = CARTESIAN_POINT ( 'NONE',  ( -10.75228648362910100, -26.64274437364854009, 37.51367750791695954 ) ) ;
#7368 = PLANE ( 'NONE',  #18950 ) ;
#7369 = CARTESIAN_POINT ( 'NONE',  ( -15.16482700510259640, -28.99999999999998224, 1.638677507916958431 ) ) ;
#7370 = CARTESIAN_POINT ( 'NONE',  ( 0.000000000000000000, -6.000000000000000000, 0.000000000000000000 ) ) ;
#7371 = ORIENTED_EDGE ( 'NONE', *, *, #6706, .F. ) ;
#7372 = EDGE_CURVE ( 'NONE', #2358, #3528, #9724, .T. ) ;
#7373 = CARTESIAN_POINT ( 'NONE',  ( -18.35725562635138886, -30.14459132904237393, 40.79882249208304046 ) ) ;
#7374 = EDGE_CURVE ( 'NONE', #13384, #3397, #18474, .T. ) ;
#7375 = AXIS2_PLACEMENT_3D ( 'NONE', #12926, #18920, #11451 ) ;
#7376 = CARTESIAN_POINT ( 'NONE',  ( -21.99999999999999289, -23.83517299489739116, 2.951177507916956433 ) ) ;
#7377 = AXIS2_PLACEMENT_3D ( 'NONE', #8614, #12830, #1166 ) ;
#7378 = CARTESIAN_POINT ( 'NONE',  ( -1.461580736456473906, 65.46158073645646880, 46.25000000109247367 ) ) ;
#7379 = CARTESIAN_POINT ( 'NONE',  ( -19.99999999999999645, -24.16482700510261949, 41.67382249208304046 ) ) ;
#7380 = CARTESIAN_POINT ( 'NONE',  ( -1.767766952966370209, 65.76776695296638309, 45.89999999999999858 ) ) ;
#7381 = VERTEX_POINT ( 'NONE', #11282 ) ;
#7382 = DIRECTION ( 'NONE',  ( 0.000000000000000000, -1.000000000000000000, 0.000000000000000000 ) ) ;
#7383 = EDGE_LOOP ( 'NONE', ( #17815, #2542 ) ) ;
#7384 = DIRECTION ( 'NONE',  ( -8.673617379884027583E-16, 1.000000000000000000, 0.000000000000000000 ) ) ;
#7385 = CARTESIAN_POINT ( 'NONE',  ( -41.00000000000000711, 53.00000000000000711, -6.000000000000001776 ) ) ;
#7386 = CARTESIAN_POINT ( 'NONE',  ( 1.767766952966369987, 65.76776695296638309, 45.00000000218494733 ) ) ;
#7387 = DIRECTION ( 'NONE',  ( 0.000000000000000000, 1.000000000000000000, 0.000000000000000000 ) ) ;
#7388 = CARTESIAN_POINT ( 'NONE',  ( 2.500000000000001776, 64.00000000000000000, 46.39999999999999858 ) ) ;
#7389 = CARTESIAN_POINT ( 'NONE',  ( 2.066987300000001859, 63.14382582708704916, 46.90000000109247225 ) ) ;
#7390 = VECTOR ( 'NONE', #534, 1000.000000000000000 ) ;
#7391 = AXIS2_PLACEMENT_3D ( 'NONE', #12584, #13957, #18578 ) ;
#7392 = PRODUCT_DEFINITION_SHAPE ( 'NONE', 'NONE',  #12552 ) ;
#7393 = DIRECTION ( 'NONE',  ( 1.000000000000000000, -0.000000000000000000, -0.000000000000000000 ) ) ;
#7394 = CARTESIAN_POINT ( 'NONE',  ( 2.500000000000002220, 62.96446609406726935, 46.34999999999999432 ) ) ;
#7395 = CARTESIAN_POINT ( 'NONE',  ( -8.528048594804062077, -42.28611686177728046, 3.000000000000000000 ) ) ;
#7396 = EDGE_CURVE ( 'NONE', #11135, #3236, #16901, .T. ) ;
#7397 = ORIENTED_EDGE ( 'NONE', *, *, #9739, .F. ) ;
#7398 = CARTESIAN_POINT ( 'NONE',  ( -19.24771351637089367, -21.35725562635142438, 8.638677507916957765 ) ) ;
#7399 = CARTESIAN_POINT ( 'NONE',  ( -17.35725562635144215, -19.58745947852648683, 19.57617750791695954 ) ) ;
#7400 = CARTESIAN_POINT ( 'NONE',  ( -1.942750718018138034, 65.20191092753520934, 45.00000000000002132 ) ) ;
#7401 = CARTESIAN_POINT ( 'NONE',  ( -13.82508104294702100, -18.95583473709188382, 6.455072492083041347 ) ) ;
#7402 = VECTOR ( 'NONE', #9618, 1000.000000000000000 ) ;
#7403 = AXIS2_PLACEMENT_3D ( 'NONE', #13840, #17169, #12740 ) ;
#7404 = CARTESIAN_POINT ( 'NONE',  ( 2.066987300000001415, 64.00000000000000000, 46.15000000109247225 ) ) ;
#7405 = CARTESIAN_POINT ( 'NONE',  ( -11.21908421996108629, -20.46040770435011069, -0.3300724920830416798 ) ) ;
#7406 = CARTESIAN_POINT ( 'NONE',  ( -11.46040770435012490, -27.78091578003888173, 11.48242750791695777 ) ) ;
#7407 = DIRECTION ( 'NONE',  ( -0.000000000000000000, 0.000000000000000000, -1.000000000000000000 ) ) ;
#7408 = DIRECTION ( 'NONE',  ( -0.000000000000000000, -1.000000000000000000, -0.000000000000000000 ) ) ;
#7409 = LINE ( 'NONE', #7307, #13733 ) ;
#7410 = DIRECTION ( 'NONE',  ( 1.000000000000000000, 0.000000000000000000, 0.000000000000000000 ) ) ;
#7411 = CARTESIAN_POINT ( 'NONE',  ( -40.00000000000000711, 110.0000000000000000, -24.49999999999999645 ) ) ;
#7412 = CARTESIAN_POINT ( 'NONE',  ( 12.55500000000001748, 0.000000000000000000, 2.500000000000000444 ) ) ;
#7413 = VECTOR ( 'NONE', #19119, 1000.000000000000000 ) ;
#7414 = ADVANCED_FACE ( 'NONE', ( #4950 ), #10906, .F. ) ;
#7415 = DIRECTION ( 'NONE',  ( -1.000000000000000000, 1.110223024625155752E-14, 0.000000000000000000 ) ) ;
#7417 = ORIENTED_EDGE ( 'NONE', *, *, #9608, .T. ) ;
#7416 = EDGE_CURVE ( 'NONE', #15605, #301, #14149, .T. ) ;
#7418 = ORIENTED_EDGE ( 'NONE', *, *, #8414, .T. ) ;
#7419 = CARTESIAN_POINT ( 'NONE',  ( -16.71081734191520596, -31.04416526290808065, 14.33007249208304046 ) ) ;
#7420 = CARTESIAN_POINT ( 'NONE',  ( 5.199999999999996625, 0.000000000000000000, 0.000000000000000000 ) ) ;
#7422 = ORIENTED_EDGE ( 'NONE', *, *, #18079, .T. ) ;
#7421 = EDGE_LOOP ( 'NONE', ( #415, #15199, #602, #4891 ) ) ;
#7423 = CARTESIAN_POINT ( 'NONE',  ( -11.99999999999999289, -24.16482700510258752, 21.32617750791695954 ) ) ;
#7424 = CARTESIAN_POINT ( 'NONE',  ( 7.500000000000005329, -38.00000000000000000, 4.500000000000000888 ) ) ;
#7425 = CARTESIAN_POINT ( 'NONE',  ( -22.04416526290809486, -22.28918265808477628, 5.142572492083038682 ) ) ;
#7426 = CARTESIAN_POINT ( 'NONE',  ( -2.066987300000001859, 64.85617417291294373, 48.70000000109247651 ) ) ;
#7427 = CARTESIAN_POINT ( 'NONE',  ( -1.035533905932738863, 61.50000000000000000, 44.65000000218494591 ) ) ;
#7428 = ORIENTED_EDGE ( 'NONE', *, *, #11864, .F. ) ;
#7429 = ORIENTED_EDGE ( 'NONE', *, *, #276, .T. ) ;
#7430 = DIRECTION ( 'NONE',  ( -1.000000000000000000, -0.000000000000000000, -0.000000000000000000 ) ) ;
#7431 = VERTEX_POINT ( 'NONE', #14046 ) ;
#7432 = ORIENTED_EDGE ( 'NONE', *, *, #132, .T. ) ;
#7433 = CARTESIAN_POINT ( 'NONE',  ( -13.25540099147408846, -20.31871257162172739, 7.657166918419680705E-13 ) ) ;
#7434 = CARTESIAN_POINT ( 'NONE',  ( -2.315774708385926139, 31.32836399182264842, 54.80336399182263563 ) ) ;
#7435 = CARTESIAN_POINT ( 'NONE',  ( 3.796994071234847710E-16, 61.93301269999999903, 48.35000000109246798 ) ) ;
#7436 = APPLICATION_CONTEXT ( 'automotive_design' ) ;
#7437 = FACE_OUTER_BOUND ( 'NONE', #390, .T. ) ;
#7438 = EDGE_CURVE ( 'NONE', #4215, #7750, #12867, .T. ) ;
#7439 = DIRECTION ( 'NONE',  ( 0.000000000000000000, 0.000000000000000000, -1.000000000000000000 ) ) ;
#7440 = EDGE_LOOP ( 'NONE', ( #16773, #18040, #8571, #15874 ) ) ;
#7442 = ORIENTED_EDGE ( 'NONE', *, *, #1738, .F. ) ;
#7441 = ORIENTED_EDGE ( 'NONE', *, *, #2003, .T. ) ;
#7443 = CARTESIAN_POINT ( 'NONE',  ( -21.99999999999999289, -23.83517299489739116, 18.70117750791695599 ) ) ;
#7444 = CARTESIAN_POINT ( 'NONE',  ( -6.528048594804060301, -45.28611686177728046, 1.500000000000000000 ) ) ;
#7445 = ORIENTED_EDGE ( 'NONE', *, *, #19337, .F. ) ;
#7446 = ORIENTED_EDGE ( 'NONE', *, *, #821, .T. ) ;
#7447 = CARTESIAN_POINT ( 'NONE',  ( -11.95583473709190514, -24.63902057219072361, 23.51757249208304401 ) ) ;
#7448 = EDGE_CURVE ( 'NONE', #13439, #2933, #1998, .T. ) ;
#7449 = DIRECTION ( 'NONE',  ( 1.000000000000000000, -0.000000000000000000, -0.000000000000000000 ) ) ;
#7450 = DIRECTION ( 'NONE',  ( 0.000000000000000000, 0.000000000000000000, 1.000000000000000000 ) ) ;
#7451 = ORIENTED_EDGE ( 'NONE', *, *, #7860, .T. ) ;
#7452 = CARTESIAN_POINT ( 'NONE',  ( -14.83517299489738761, -20.99999999999997513, -0.9863224920830401254 ) ) ;
#7453 = CARTESIAN_POINT ( 'NONE',  ( -1.040834085586084257E-14, 29.74264068711926257, 56.74264068711929809 ) ) ;
#7454 = EDGE_LOOP ( 'NONE', ( #4188, #7251, #6313, #9306 ) ) ;
#7455 = CARTESIAN_POINT ( 'NONE',  ( 2.500000000000001776, 64.00000000000000000, 49.99999999999999289 ) ) ;
#7456 = ORIENTED_EDGE ( 'NONE', *, *, #12764, .F. ) ;
#7457 = DIRECTION ( 'NONE',  ( -0.000000000000000000, 1.000000000000000000, -0.000000000000000000 ) ) ;
#7458 = PLANE ( 'NONE',  #1420 ) ;
#7459 = CARTESIAN_POINT ( 'NONE',  ( 5.799999999999985612, 29.47747564417429444, 56.65425233947099315 ) ) ;
#7460 = APPLICATION_PROTOCOL_DEFINITION ( 'draft international standard', 'automotive_design', 1998, #10429 ) ;
#7461 = DIRECTION ( 'NONE',  ( -0.000000000000000000, -1.000000000000000000, -0.000000000000000000 ) ) ;
#7462 = VECTOR ( 'NONE', #6925, 1000.000000000000000 ) ;
#7463 = CARTESIAN_POINT ( 'NONE',  ( -2.500000000000001776, 64.00000000000000000, 49.99999999999999289 ) ) ;
#7464 = EDGE_CURVE ( 'NONE', #5915, #11555, #431, .T. ) ;
#7465 = CARTESIAN_POINT ( 'NONE',  ( -1.040834085586084257E-14, -42.00099999999996214, -15.00100000000031208 ) ) ;
#7466 = EDGE_CURVE ( 'NONE', #9583, #6113, #11189, .T. ) ;
#7467 = CARTESIAN_POINT ( 'NONE',  ( -16.17491895705301275, -18.95583473709189803, 19.79492750791695954 ) ) ;
#7468 = CARTESIAN_POINT ( 'NONE',  ( 1.300000000000000044, 1.478016689125442484, -1.626303258728256651E-15 ) ) ;
#7469 = VERTEX_POINT ( 'NONE', #12759 ) ;
#7470 = CARTESIAN_POINT ( 'NONE',  ( -21.99999999999999289, -24.16482700510262305, 41.67382249208304756 ) ) ;
#7471 = CARTESIAN_POINT ( 'NONE',  ( 1.461580736456473684, 65.46158073645646880, 46.05000000109246372 ) ) ;
#7472 = CARTESIAN_POINT ( 'NONE',  ( -12.31951028609536536, -25.35725562635139596, 2.736322492083043123 ) ) ;
#7473 = AXIS2_PLACEMENT_3D ( 'NONE', #7481, #17679, #1318 ) ;
#7474 = CARTESIAN_POINT ( 'NONE',  ( -40.00000000000000711, 53.00000000000000711, -5.000000000000000888 ) ) ;
#7475 = VERTEX_POINT ( 'NONE', #3372 ) ;
#7476 = CARTESIAN_POINT ( 'NONE',  ( -37.50000000000002132, -6.000000000000000000, 24.99999999999998224 ) ) ;
#7477 = ORIENTED_EDGE ( 'NONE', *, *, #11864, .T. ) ;
#7478 = CARTESIAN_POINT ( 'NONE',  ( -41.00000000000000711, 53.00000000000000711, -30.99999999999999645 ) ) ;
#7479 = FACE_OUTER_BOUND ( 'NONE', #1600, .T. ) ;
#7480 = DIRECTION ( 'NONE',  ( 0.000000000000000000, 0.000000000000000000, 1.000000000000000000 ) ) ;
#7481 = CARTESIAN_POINT ( 'NONE',  ( 10.71950000000001424, 0.000000000000000000, 0.000000000000000000 ) ) ;
#7482 = FACE_BOUND ( 'NONE', #4214, .T. ) ;
#7483 = CARTESIAN_POINT ( 'NONE',  ( 0.8561741729129471734, 61.93301270000000613, 46.00000000109246656 ) ) ;
#7484 = VECTOR ( 'NONE', #5482, 1000.000000000000000 ) ;
#7485 = EDGE_CURVE ( 'NONE', #16704, #19125, #525, .T. ) ;
#7486 = CARTESIAN_POINT ( 'NONE',  ( -32.50000000000000000, 53.00000000000000711, 12.35000000000001386 ) ) ;
#7487 = CARTESIAN_POINT ( 'NONE',  ( -1.767766952966369765, 62.23223304703363112, 47.69999999999999574 ) ) ;
#7488 = LINE ( 'NONE', #9250, #11133 ) ;
#7489 = VECTOR ( 'NONE', #1264, 1000.000000000000000 ) ;
#7490 = EDGE_LOOP ( 'NONE', ( #10763, #8230, #3208, #8162 ) ) ;
#7491 =( BOUNDED_CURVE ( )  B_SPLINE_CURVE ( 2, ( #1824, #10731, #18301, #7609, #16727, #1363, #2824, #16630, #15348 ),
 .UNSPECIFIED., .F., .F. ) 
 B_SPLINE_CURVE_WITH_KNOTS ( ( 3, 2, 2, 2, 3 ),
 ( 0.7142857142857141906, 0.7321428571428569843, 0.7500000000000000000, 0.7678571428571429047, 0.7857142857142856984 ),
 .UNSPECIFIED. ) 
 CURVE ( )  GEOMETRIC_REPRESENTATION_ITEM ( )  RATIONAL_B_SPLINE_CURVE ( ( 1.000000000000000444, 0.9238795325112862944, 1.000000000000000000, 0.9238795325112867385, 1.000000000000000000, 0.9238795325112867385, 1.000000000000000000, 0.9238795325112867385, 1.000000000000000000 ) ) 
 REPRESENTATION_ITEM ( '' )  );
#7492 = CARTESIAN_POINT ( 'NONE',  ( -44.99999999999998579, -3.000000000000002665, -55.00000000000000000 ) ) ;
#7493 = CARTESIAN_POINT ( 'NONE',  ( -15.16482700510259640, -28.99999999999998224, 1.638677507916958431 ) ) ;
#7494 = CARTESIAN_POINT ( 'NONE',  ( -18.78091578003889950, -27.53959229564985378, 12.79492750791695421 ) ) ;
#7495 = CARTESIAN_POINT ( 'NONE',  ( -1.035533905932738641, 66.50000000000000000, 49.15000000218494591 ) ) ;
#7496 = CARTESIAN_POINT ( 'NONE',  ( -16.17491895705296656, -29.04416526290807710, 9.080072492083036906 ) ) ;
#7497 = VECTOR ( 'NONE', #12578, 1000.000000000000227 ) ;
#7498 = CARTESIAN_POINT ( 'NONE',  ( -1.461580736456473462, 62.53841926354353120, 45.05000000109246372 ) ) ;
#7499 = CARTESIAN_POINT ( 'NONE',  ( -17.68048971390461688, -25.35725562635141372, 39.26367750791696665 ) ) ;
#7500 = PLANE ( 'NONE',  #1244 ) ;
#7501 = CARTESIAN_POINT ( 'NONE',  ( -16.17491895705301275, -18.95583473709189448, 4.044927507916959541 ) ) ;
#7502 = VECTOR ( 'NONE', #6697, 1000.000000000000000 ) ;
#7503 = CARTESIAN_POINT ( 'NONE',  ( -0.1250000000000104083, 25.46464466094064250, 60.66708332270462734 ) ) ;
#7504 = VECTOR ( 'NONE', #11915, 1000.000000000000000 ) ;
#7505 = EDGE_CURVE ( 'NONE', #1057, #6748, #5506, .T. ) ;
#7506 = DIRECTION ( 'NONE',  ( 0.000000000000000000, 0.000000000000000000, 1.000000000000000000 ) ) ;
#7507 = DIRECTION ( 'NONE',  ( 3.826732013112564095E-16, -1.000000000000000000, -1.632680918566406793E-16 ) ) ;
#7508 = CARTESIAN_POINT ( 'NONE',  ( 2.315774708385941683, 31.50514068711926541, 54.98014068711930236 ) ) ;
#7509 = VECTOR ( 'NONE', #4001, 1000.000000000000000 ) ;
#7510 = CARTESIAN_POINT ( 'NONE',  ( -2.066987300000001415, 64.00000000000000000, 45.75000000109247367 ) ) ;
#7511 = CARTESIAN_POINT ( 'NONE',  ( 0.000000000000000000, 52.00000000000000711, -50.00000000000000000 ) ) ;
#7512 = AXIS2_PLACEMENT_3D ( 'NONE', #17586, #5626, #1317 ) ;
#7513 = CARTESIAN_POINT ( 'NONE',  ( -4.012830983233701687, 26.60336399182265055, 59.52836399182262994 ) ) ;
#7514 = ORIENTED_EDGE ( 'NONE', *, *, #8104, .T. ) ;
#7515 = EDGE_CURVE ( 'NONE', #7522, #8981, #4099, .T. ) ;
#7516 = ORIENTED_EDGE ( 'NONE', *, *, #14558, .T. ) ;
#7517 = CARTESIAN_POINT ( 'NONE',  ( -13.28918265808478694, -16.95583473709189093, 22.20507249208304046 ) ) ;
#7518 = CIRCLE ( 'NONE', #15654, 2.999999999999999112 ) ;
#7519 =( LENGTH_UNIT ( ) NAMED_UNIT ( * ) SI_UNIT ( .MILLI., .METRE. ) );
#7520 = DIRECTION ( 'NONE',  ( 0.000000000000000000, 0.000000000000000000, -1.000000000000000000 ) ) ;
#7522 = VERTEX_POINT ( 'NONE', #2375 ) ;
#7521 = ORIENTED_EDGE ( 'NONE', *, *, #8879, .F. ) ;
#7523 = CARTESIAN_POINT ( 'NONE',  ( -16.64274437364856496, -26.51566270880199738, 12.57617750791695954 ) ) ;
#7524 = DIRECTION ( 'NONE',  ( 0.000000000000000000, 0.000000000000000000, 1.000000000000000000 ) ) ;
#7525 = CARTESIAN_POINT ( 'NONE',  ( -11.35725562635139418, -29.97976432393972601, 3.173822492083039126 ) ) ;
#7526 = CARTESIAN_POINT ( 'NONE',  ( -1.767766952966370209, 65.76776695296638309, 48.29999999999999716 ) ) ;
#7527 = CARTESIAN_POINT ( 'NONE',  ( 2.500000000000001776, 65.03553390593273775, 45.75000000218494023 ) ) ;
#7528 = ORIENTED_EDGE ( 'NONE', *, *, #4353, .F. ) ;
#7529 = ORIENTED_EDGE ( 'NONE', *, *, #2786, .T. ) ;
#7530 = DIRECTION ( 'NONE',  ( 0.000000000000000000, 0.000000000000000000, 1.000000000000000000 ) ) ;
#7531 = DIRECTION ( 'NONE',  ( 0.000000000000000000, 0.7071067811865452413, 0.7071067811865497932 ) ) ;
#7532 = AXIS2_PLACEMENT_3D ( 'NONE', #4590, #1446, #19383 ) ;
#7533 = ORIENTED_EDGE ( 'NONE', *, *, #16694, .F. ) ;
#7534 = DIRECTION ( 'NONE',  ( 0.000000000000000000, -0.7071067811865455743, -0.7071067811865495711 ) ) ;
#7535 = LINE ( 'NONE', #16661, #5004 ) ;
#7536 = VECTOR ( 'NONE', #12560, 1000.000000000000000 ) ;
#7537 = CARTESIAN_POINT ( 'NONE',  ( -1.461580736456473462, 62.53841926354353120, 46.65000000109247225 ) ) ;
#7538 = DIRECTION ( 'NONE',  ( 1.000000000000000000, 0.000000000000000000, 0.000000000000000000 ) ) ;
#7539 = VECTOR ( 'NONE', #6675, 1000.000000000000000 ) ;
#7540 = DIRECTION ( 'NONE',  ( -1.000000000000000000, -0.000000000000000000, -0.000000000000000000 ) ) ;
#7541 = ORIENTED_EDGE ( 'NONE', *, *, #17150, .F. ) ;
#7543 = ORIENTED_EDGE ( 'NONE', *, *, #7625, .F. ) ;
#7542 = ORIENTED_EDGE ( 'NONE', *, *, #16757, .T. ) ;
#7544 = CARTESIAN_POINT ( 'NONE',  ( -20.00369391078762860, -18.75498260482333279, 14.10742750791695777 ) ) ;
#7545 = DIRECTION ( 'NONE',  ( 0.000000000000000000, -0.000000000000000000, -1.000000000000000000 ) ) ;
#7546 = AXIS2_PLACEMENT_3D ( 'NONE', #14470, #755, #2322 ) ;
#7547 = VERTEX_POINT ( 'NONE', #18852 ) ;
#7548 = EDGE_LOOP ( 'NONE', ( #12247, #18848, #1610, #13815 ) ) ;
#7549 = CARTESIAN_POINT ( 'NONE',  ( -12.92450931948790149, -21.68318583509881137, 17.39257249208304046 ) ) ;
#7550 = AXIS2_PLACEMENT_3D ( 'NONE', #7615, #4581, #17808 ) ;
#7551 = DIRECTION ( 'NONE',  ( -0.000000000000000000, -1.000000000000000000, -0.000000000000000000 ) ) ;
#7552 = VERTEX_POINT ( 'NONE', #899 ) ;
#7553 = CARTESIAN_POINT ( 'NONE',  ( -16.35725562635142794, -21.31951028609535470, 19.57617750791696309 ) ) ;
#7554 = CLOSED_SHELL ( 'NONE', ( #16065, #10995, #8448, #18271, #14203, #8310, #8010, #9034, #7245, #907, #13847, #4379, #9352, #3043, #10698, #3891, #13246, #13345, #5432, #9714, #7837, #10064, #8638, #10035, #7954, #3255 ) ) ;
#7555 = DIRECTION ( 'NONE',  ( 0.000000000000000000, 0.7071067811865493491, -0.7071067811865457964 ) ) ;
#7556 = EDGE_LOOP ( 'NONE', ( #9903, #4563, #6387, #6448 ) ) ;
#7557 = DIRECTION ( 'NONE',  ( 1.000000000000000000, -0.000000000000000000, -0.000000000000000000 ) ) ;
#7558 = PRODUCT_DEFINITION_SHAPE ( 'NONE', 'NONE',  #19410 ) ;
#7559 = ORIENTED_EDGE ( 'NONE', *, *, #18383, .T. ) ;
#7560 = FACE_OUTER_BOUND ( 'NONE', #16967, .T. ) ;
#7561 = DIRECTION ( 'NONE',  ( 0.000000000000000000, 0.000000000000000000, 1.000000000000000000 ) ) ;
#7562 = CARTESIAN_POINT ( 'NONE',  ( -24.00000000000000000, 52.00000000000000711, -50.00000000000000000 ) ) ;
#7563 = CIRCLE ( 'NONE', #47, 2.649999999999999467 ) ;
#7564 = APPLICATION_PROTOCOL_DEFINITION ( 'draft international standard', 'automotive_design', 1998, #4057 ) ;
#7565 = LINE ( 'NONE', #4535, #63 ) ;
#7566 = EDGE_CURVE ( 'NONE', #12231, #9848, #9997, .T. ) ;
#7567 = EDGE_CURVE ( 'NONE', #11531, #5928, #15807, .T. ) ;
#7568 = AXIS2_PLACEMENT_3D ( 'NONE', #16979, #6584, #1975 ) ;
#7569 = CARTESIAN_POINT ( 'NONE',  ( -14.83517299489739649, -18.99999999999997868, 35.76367750791695954 ) ) ;
#7570 = FACE_OUTER_BOUND ( 'NONE', #11923, .T. ) ;
#7572 = EDGE_CURVE ( 'NONE', #292, #18125, #2753, .T. ) ;
#7571 = CARTESIAN_POINT ( 'NONE',  ( -9.955834737091912245, -22.82508104294696594, 10.60742750791695777 ) ) ;
#7573 = LINE ( 'NONE', #1303, #3345 ) ;
#7574 = ORIENTED_EDGE ( 'NONE', *, *, #17493, .F. ) ;
#7575 = CARTESIAN_POINT ( 'NONE',  ( -12.35725562635140307, -28.24771351637085459, 13.67382249208304223 ) ) ;
#7576 = EDGE_CURVE ( 'NONE', #16562, #10557, #9437, .T. ) ;
#7577 = AXIS2_PLACEMENT_3D ( 'NONE', #19332, #219, #6204 ) ;
#7578 = CARTESIAN_POINT ( 'NONE',  ( 4.012354697599942455, 32.70432772728315740, 53.78000129688596331 ) ) ;
#7579 = CARTESIAN_POINT ( 'NONE',  ( -18.04416526290808775, -23.36097942780924441, 15.64257249208304579 ) ) ;
#7580 = AXIS2_PLACEMENT_3D ( 'NONE', #5770, #1262, #15253 ) ;
#7581 = CYLINDRICAL_SURFACE ( 'NONE', #2816, 2.500000000000001776 ) ;
#7582 = ORIENTED_EDGE ( 'NONE', *, *, #17526, .T. ) ;
#7583 = CARTESIAN_POINT ( 'NONE',  ( 0.000000000000000000, 64.00000000000000000, 49.99999999999999289 ) ) ;
#7584 = ORIENTED_EDGE ( 'NONE', *, *, #17230, .T. ) ;
#7585 = FACE_OUTER_BOUND ( 'NONE', #18512, .T. ) ;
#7586 = EDGE_CURVE ( 'NONE', #7101, #3717, #6879, .T. ) ;
#7587 = DIRECTION ( 'NONE',  ( 1.000000000000000000, 0.000000000000000000, 9.251858538542970348E-17 ) ) ;
#7588 = CARTESIAN_POINT ( 'NONE',  ( 0.1499999999999973577, 0.000000000000000000, 0.000000000000000000 ) ) ;
#7589 = PLANE ( 'NONE',  #14408 ) ;
#7590 = CARTESIAN_POINT ( 'NONE',  ( 2.066987300000001859, 63.14382582708704916, 45.30000000109246372 ) ) ;
#7591 = DIRECTION ( 'NONE',  ( -1.000000000000000000, -0.000000000000000000, -0.000000000000000000 ) ) ;
#7592 = EDGE_CURVE ( 'NONE', #14201, #4122, #17367, .T. ) ;
#7593 = CARTESIAN_POINT ( 'NONE',  ( 4.592425496802577917E-16, 61.50000000000000000, 45.39999999999999858 ) ) ;
#7594 = CARTESIAN_POINT ( 'NONE',  ( 14.99999999999998579, 73.00000000000001421, 23.99999999999997158 ) ) ;
#7595 = ORIENTED_EDGE ( 'NONE', *, *, #4746, .F. ) ;
#7596 = DIRECTION ( 'NONE',  ( 0.000000000000000000, 0.000000000000000000, 1.000000000000000000 ) ) ;
#7597 = CARTESIAN_POINT ( 'NONE',  ( -20.04416526290808065, -25.17491895705300209, 13.23242750791695777 ) ) ;
#7598 = CARTESIAN_POINT ( 'NONE',  ( -13.49542703274178379, -19.04416526290806289, 14.98242750791695777 ) ) ;
#7599 = CARTESIAN_POINT ( 'NONE',  ( -0.7262361202807413596, 66.33061197500782669, 45.00000000000001421 ) ) ;
#7600 = CARTESIAN_POINT ( 'NONE',  ( -18.35725562635138886, -30.14459132904237393, 40.79882249208304046 ) ) ;
#7601 = EDGE_CURVE ( 'NONE', #4696, #13296, #5354, .T. ) ;
#7602 = EDGE_CURVE ( 'NONE', #7381, #10051, #15899, .T. ) ;
#7603 = CARTESIAN_POINT ( 'NONE',  ( 0.8561741729129472844, 61.93301270000000613, 45.20000000109248361 ) ) ;
#7604 = CARTESIAN_POINT ( 'NONE',  ( -15.16482700510260706, -26.99999999999998579, 38.38867750791695954 ) ) ;
#7605 = EDGE_CURVE ( 'NONE', #7955, #8804, #17460, .T. ) ;
#7606 = CARTESIAN_POINT ( 'NONE',  ( -24.00000000000000711, 53.00000000000000711, -38.50000000000000711 ) ) ;
#7607 = CARTESIAN_POINT ( 'NONE',  ( -10.75228648362910100, -26.64274437364854009, 16.51367750791695954 ) ) ;
#7608 = CARTESIAN_POINT ( 'NONE',  ( -32.50000000000000000, 53.00000000000000711, -32.35000000000000853 ) ) ;
#7609 = CARTESIAN_POINT ( 'NONE',  ( -1.035533905932738641, 66.50000000000000000, 45.84999999999998721 ) ) ;
#7610 = EDGE_CURVE ( 'NONE', #16061, #17639, #10872, .T. ) ;
#7611 = CARTESIAN_POINT ( 'NONE',  ( -1.265664690411616068E-16, 66.06698730000000808, 47.15000000109247225 ) ) ;
#7612 = PLANE ( 'NONE',  #19360 ) ;
#7613 = PLANE ( 'NONE',  #13500 ) ;
#7614 = CARTESIAN_POINT ( 'NONE',  ( -0.8561741729129466183, 61.93301270000000613, 45.90000000109247225 ) ) ;
#7615 = CARTESIAN_POINT ( 'NONE',  ( -14.99999999999999645, 73.00000000000001421, 23.99999999999997868 ) ) ;
#7616 = DIRECTION ( 'NONE',  ( -1.000000000000000000, -0.000000000000000000, -0.000000000000000000 ) ) ;
#7617 =( BOUNDED_CURVE ( )  B_SPLINE_CURVE ( 2, ( #490, #9500, #4820, #7652, #3531, #583, #3239, #295, #12147, #13913, #13718, #203, #15295, #5008, #12345, #15105, #7754, #12443, #13821, #3341, #15489, #1771, #16770, #1675, #6575, #2058, #6282, #5110, #1966, #9309, #6476, #16571, #9116, #13618, #6191, #10678, #7950, #12253, #10967, #9212, #18249, #10768, #15203, #1867, #7853, #399, #6382, #18343, #4913, #16867, #3430, #9403, #15397, #11405, #9932, #15650, #6727, #14459, #837, #2402, #5260, #11500, #745, #3789, #2219, #17401, #17220, #3688, #18782, #8482, #15838, #18602, #11214, #15929, #17312, #6818, #12975, #15748, #9756, #2311, #931, #18973, #8295, #4066, #5447, #12785, #3975, #17490, #1032, #2592, #16033, #12608, #2493, #14267, #7006, #11128, #5358, #8573, #9658, #5544, #10034 ),
 .UNSPECIFIED., .F., .F. ) 
 B_SPLINE_CURVE_WITH_KNOTS ( ( 3, 2, 2, 2, 2, 2, 2, 2, 2, 2, 2, 2, 2, 2, 2, 2, 2, 2, 2, 2, 2, 2, 2, 2, 2, 2, 2, 2, 2, 2, 2, 2, 2, 2, 2, 2, 2, 2, 2, 2, 2, 2, 2, 2, 2, 2, 2, 2, 2, 2, 3 ),
 ( 0.000000000000000000, 0.01785714285714285615, 0.03571428571428571230, 0.05357142857142856845, 0.07142857142857142461, 0.08928571428571428770, 0.1071428571428571369, 0.1250000000000000000, 0.1428571428571428492, 0.1607142857142857262, 0.1785714285714285754, 0.1964285714285714246, 0.2142857142857142738, 0.2321428571428571508, 0.2500000000000000000, 0.2678571428571428492, 0.2857142857142856984, 0.3035714285714285476, 0.3214285714285714524, 0.3392857142857143016, 0.3571428571428571508, 0.3750000000000000000, 0.3928571428571428492, 0.4107142857142856984, 0.4285714285714285476, 0.4464285714285714524, 0.4642857142857143016, 0.4821428571428571508, 0.5000000000000000000, 0.5178571428571429047, 0.5357142857142856984, 0.5535714285714286031, 0.5714285714285713969, 0.5892857142857143016, 0.6071428571428570953, 0.6250000000000000000, 0.6428571428571429047, 0.6607142857142856984, 0.6785714285714286031, 0.6964285714285715079, 0.7142857142857143016, 0.7321428571428570953, 0.7500000000000000000, 0.7678571428571429047, 0.7857142857142856984, 0.8035714285714286031, 0.8214285714285713969, 0.8392857142857143016, 0.8571428571428570953, 0.8750000000000000000, 0.8928571428571429047 ),
 .UNSPECIFIED. ) 
 CURVE ( )  GEOMETRIC_REPRESENTATION_ITEM ( )  RATIONAL_B_SPLINE_CURVE ( ( 1.000000000000000000, 0.9238795325112867385, 1.000000000000000000, 0.9238795325112867385, 1.000000000000000000, 0.9238795325112867385, 1.000000000000000000, 0.9238795325112867385, 1.000000000000000000, 0.9238795325112867385, 1.000000000000000000, 0.9238795325112867385, 1.000000000000000000, 0.9238795325112867385, 1.000000000000000000, 0.9238795325112867385, 1.000000000000000000, 0.9238795325112867385, 1.000000000000000000, 0.9238795325112867385, 1.000000000000000000, 0.9238795325112867385, 1.000000000000000000, 0.9238795325112867385, 1.000000000000000000, 0.9238795325112867385, 1.000000000000000000, 0.9238795325112867385, 1.000000000000000000, 0.9238795325112867385, 1.000000000000000000, 0.9238795325112867385, 1.000000000000000000, 0.9238795325112867385, 1.000000000000000000, 0.9238795325112867385, 1.000000000000000000, 0.9238795325112867385, 1.000000000000000000, 0.9238795325112867385, 1.000000000000000000, 0.9238795325112867385, 1.000000000000000000, 0.9238795325112867385, 1.000000000000000000, 0.9238795325112867385, 1.000000000000000000, 0.9238795325112867385, 1.000000000000000000, 0.9238795325112867385, 1.000000000000000000, 0.9238795325112867385, 1.000000000000000000, 0.9238795325112867385, 1.000000000000000000, 0.9238795325112867385, 1.000000000000000000, 0.9238795325112867385, 1.000000000000000000, 0.9238795325112867385, 1.000000000000000000, 0.9238795325112867385, 1.000000000000000000, 0.9238795325112867385, 1.000000000000000000, 0.9238795325112867385, 1.000000000000000000, 0.9238795325112867385, 1.000000000000000000, 0.9238795325112867385, 1.000000000000000000, 0.9238795325112867385, 1.000000000000000000, 0.9238795325112867385, 1.000000000000000000, 0.9238795325112867385, 1.000000000000000000, 0.9238795325112867385, 1.000000000000000000, 0.9238795325112867385, 1.000000000000000000, 0.9238795325112867385, 1.000000000000000000, 0.9238795325112867385, 1.000000000000000000, 0.9238795325112867385, 1.000000000000000000, 0.9238795325112867385, 1.000000000000000000, 0.9238795325112867385, 1.000000000000000000, 0.9238795325112867385, 1.000000000000000000, 0.9238795325112867385, 1.000000000000000000, 0.9238795325112867385, 1.000000000000000000, 0.9238795325112867385, 1.000000000000000000, 0.9238795325112867385, 1.000000000000000000 ) ) 
 REPRESENTATION_ITEM ( '' )  );
#7618 = CARTESIAN_POINT ( 'NONE',  ( -1.040834085586084257E-14, 29.03553390593270578, 56.03553390593273775 ) ) ;
#7619 = ORIENTED_EDGE ( 'NONE', *, *, #13231, .T. ) ;
#7620 = ORIENTED_EDGE ( 'NONE', *, *, #18620, .T. ) ;
#7621 = CARTESIAN_POINT ( 'NONE',  ( -14.83517299489734853, -30.99999999999998224, 14.11132249208304046 ) ) ;
#7622 = CARTESIAN_POINT ( 'NONE',  ( 1.035533905932738197, 66.50000000000000000, 47.34999999999998721 ) ) ;
#7624 = EDGE_LOOP ( 'NONE', ( #9776, #16715, #2716, #13193 ) ) ;
#7623 = ORIENTED_EDGE ( 'NONE', *, *, #11929, .T. ) ;
#7625 = EDGE_CURVE ( 'NONE', #10268, #8851, #10191, .T. ) ;
#7626 = CARTESIAN_POINT ( 'NONE',  ( -12.48433729119798130, -25.64274437364855075, 16.51367750791695954 ) ) ;
#7627 = CARTESIAN_POINT ( 'NONE',  ( -2.066987300000001415, 64.00000000000000000, 49.55000000109247082 ) ) ;
#7628 = CARTESIAN_POINT ( 'NONE',  ( -13.28918265808478694, -16.95583473709189093, 1.205072492083039126 ) ) ;
#7629 = CARTESIAN_POINT ( 'NONE',  ( -1.461580736456473462, 62.53841926354353120, 48.05000000109247082 ) ) ;
#7630 = CARTESIAN_POINT ( 'NONE',  ( -0.8561741729129465073, 61.93301270000000613, 46.50000000109247367 ) ) ;
#7631 = VERTEX_POINT ( 'NONE', #10094 ) ;
#7632 = ORIENTED_EDGE ( 'NONE', *, *, #15381, .F. ) ;
#7633 = DIRECTION ( 'NONE',  ( 1.000000000000000000, 0.000000000000000000, 0.000000000000000000 ) ) ;
#7634 = CARTESIAN_POINT ( 'NONE',  ( -25.00000000000000711, 53.00000000000000711, 14.50000000000000000 ) ) ;
#7635 = ORIENTED_EDGE ( 'NONE', *, *, #9137, .T. ) ;
#7636 = CARTESIAN_POINT ( 'NONE',  ( -15.00000000000000000, -17.18313764714974923, -16.36466261444977377 ) ) ;
#7637 = DIRECTION ( 'NONE',  ( -0.5773502691896360561, -0.8164965809277188180, 0.000000000000000000 ) ) ;
#7638 = CARTESIAN_POINT ( 'NONE',  ( 3.796994071234847710E-16, 61.93301269999999903, 46.75000000109246656 ) ) ;
#7639 = PRODUCT_DEFINITION ( 'UNKNOWN', '', #2355, #19042 ) ;
#7640 = CARTESIAN_POINT ( 'NONE',  ( -41.00000000000000711, 53.00000000000000711, -44.00000000000000000 ) ) ;
#7641 = DIRECTION ( 'NONE',  ( 0.7071067811865389130, -0.5000000000000073275, 0.5000000000000048850 ) ) ;
#7642 = EDGE_LOOP ( 'NONE', ( #16300, #11232, #3427, #3786, #12347 ) ) ;
#7644 = ORIENTED_EDGE ( 'NONE', *, *, #17150, .T. ) ;
#7643 = ORIENTED_EDGE ( 'NONE', *, *, #16772, .F. ) ;
#7645 = CARTESIAN_POINT ( 'NONE',  ( -7.999999999999996447, -24.16482700510256976, 10.82617750791695599 ) ) ;
#7646 = DIRECTION ( 'NONE',  ( 1.000000000000000000, 0.000000000000000000, 0.000000000000000000 ) ) ;
#7647 = ORIENTED_EDGE ( 'NONE', *, *, #18637, .F. ) ;
#7648 = VERTEX_POINT ( 'NONE', #2653 ) ;
#7649 = EDGE_CURVE ( 'NONE', #2217, #1789, #8635, .T. ) ;
#7650 = CARTESIAN_POINT ( 'NONE',  ( -11.99999999999999289, -23.83517299489735564, 12.79882249208304223 ) ) ;
#7651 = AXIS2_PLACEMENT_3D ( 'NONE', #10717, #434, #10809 ) ;
#7652 = CARTESIAN_POINT ( 'NONE',  ( -0.8561741729129461742, 66.06698730000000808, 49.40000000109247225 ) ) ;
#7653 = CARTESIAN_POINT ( 'NONE',  ( -2.492551403682565780, 31.38014068711928672, 55.10514068711927393 ) ) ;
#7654 = ORIENTED_EDGE ( 'NONE', *, *, #9639, .F. ) ;
#7655 = CARTESIAN_POINT ( 'NONE',  ( -15.63902057219076269, -20.95583473709189448, 14.54492750791695954 ) ) ;
#7656 = FACE_OUTER_BOUND ( 'NONE', #7717, .T. ) ;
#7657 = ORIENTED_EDGE ( 'NONE', *, *, #18637, .T. ) ;
#7658 = FACE_OUTER_BOUND ( 'NONE', #2173, .T. ) ;
#7659 = EDGE_LOOP ( 'NONE', ( #13710, #4811, #8605, #1356 ) ) ;
#7660 = CARTESIAN_POINT ( 'NONE',  ( -41.00000000000000711, 53.00000000000000711, -5.000000000000000888 ) ) ;
#7661 = CARTESIAN_POINT ( 'NONE',  ( 2.500000000000001776, 64.00000000000000000, 47.19999999999999574 ) ) ;
#7662 = LINE ( 'NONE', #3149, #8797 ) ;
#7663 = ITEM_DEFINED_TRANSFORMATION ( 'NONE', 'NONE', #5470,  #1791 ) ;
#7664 = CARTESIAN_POINT ( 'NONE',  ( 2.500000000000001776, 64.00000000000000000, 48.90000000218494591 ) ) ;
#7665 = DIRECTION ( 'NONE',  ( -0.000000000000000000, -0.000000000000000000, -1.000000000000000000 ) ) ;
#7666 = PRESENTATION_LAYER_ASSIGNMENT (  '', '', ( #7343 ) ) ;
#7667 = CARTESIAN_POINT ( 'NONE',  ( -19.95583473709191580, -22.49542703274176603, 39.91992750791695954 ) ) ;
#7668 = AXIS2_PLACEMENT_3D ( 'NONE', #10509, #13357, #1703 ) ;
#7669 = CARTESIAN_POINT ( 'NONE',  ( 24.99999999999998579, 0.000000000000000000, 47.49999999999997868 ) ) ;
#7670 = CARTESIAN_POINT ( 'NONE',  ( -11.21908421996108629, -20.46040770435011069, 10.16992750791695244 ) ) ;
#7671 = CARTESIAN_POINT ( 'NONE',  ( -41.00000000000000711, 110.0000000000000000, -45.00000000000000000 ) ) ;
#7672 = ORIENTED_EDGE ( 'NONE', *, *, #15260, .F. ) ;
#7673 = UNCERTAINTY_MEASURE_WITH_UNIT (LENGTH_MEASURE( 1.000000000000000082E-05 ), #15837, 'distance_accuracy_value', 'NONE');
#7674 = CARTESIAN_POINT ( 'NONE',  ( -15.16482700510263371, -18.99999999999997868, 11.48632249208304046 ) ) ;
#7675 = CARTESIAN_POINT ( 'NONE',  ( 0.000000000000000000, 0.000000000000000000, -50.00000000000000000 ) ) ;
#7676 = CARTESIAN_POINT ( 'NONE',  ( -15.63902057219073605, -27.04416526290807710, 24.83007249208304046 ) ) ;
#7677 = PRODUCT_DEFINITION_FORMATION_WITH_SPECIFIED_SOURCE ( 'ANY', '', #1449, .NOT_KNOWN. ) ;
#7678 = DIRECTION ( 'NONE',  ( -0.000000000000000000, -0.000000000000000000, -1.000000000000000000 ) ) ;
#7679 = ORIENTED_EDGE ( 'NONE', *, *, #13702, .T. ) ;
#7680 = VECTOR ( 'NONE', #12849, 1000.000000000000000 ) ;
#7681 = DIRECTION ( 'NONE',  ( -0.000000000000000000, -0.000000000000000000, -1.000000000000000000 ) ) ;
#7682 = EDGE_LOOP ( 'NONE', ( #15955, #13281, #11797, #6473, #12625 ) ) ;
#7683 = DIRECTION ( 'NONE',  ( 0.000000000000000000, -1.026972870230479989E-15, -1.000000000000000000 ) ) ;
#7684 = CARTESIAN_POINT ( 'NONE',  ( 24.99999999999998579, 0.000000000000000000, 47.49999999999997868 ) ) ;
#7685 = CARTESIAN_POINT ( 'NONE',  ( -41.00000000000000711, 110.0000000000000000, 1.500000000000001332 ) ) ;
#7686 = CARTESIAN_POINT ( 'NONE',  ( 2.066987300000001415, 64.00000000000000000, 47.75000000109246656 ) ) ;
#7687 = EDGE_CURVE ( 'NONE', #2714, #13223, #13170, .T. ) ;
#7688 = CARTESIAN_POINT ( 'NONE',  ( 4.012830983233625304, 26.60336399182260791, 59.52836399182266547 ) ) ;
#7689 = PLANE ( 'NONE',  #10363 ) ;
#7690 = DIRECTION ( 'NONE',  ( 0.000000000000000000, 0.000000000000000000, -1.000000000000000000 ) ) ;
#7691 = VECTOR ( 'NONE', #479, 1000.000000000000000 ) ;
#7692 = VECTOR ( 'NONE', #16531, 1000.000000000000000 ) ;
#7693 = UNCERTAINTY_MEASURE_WITH_UNIT (LENGTH_MEASURE( 1.000000000000000082E-05 ), #8983, 'distance_accuracy_value', 'NONE');
#7694 = ORIENTED_EDGE ( 'NONE', *, *, #12293, .F. ) ;
#7695 = CARTESIAN_POINT ( 'NONE',  ( 29.99999999999999645, 2.999999999999999112, 0.000000000000000000 ) ) ;
#7696 = CARTESIAN_POINT ( 'NONE',  ( -18.53959229564986799, -20.21908421996107563, 24.60742750791695954 ) ) ;
#7697 = CARTESIAN_POINT ( 'NONE',  ( -2.500000000000001776, 64.00000000000000000, 48.50000000218494023 ) ) ;
#7698 = EDGE_CURVE ( 'NONE', #11751, #834, #8188, .T. ) ;
#7699 = CARTESIAN_POINT ( 'NONE',  ( -10.04416526290808953, -22.49542703274172695, 17.83007249208303691 ) ) ;
#7700 = CARTESIAN_POINT ( 'NONE',  ( -2.066987300000001859, 64.85617417291294373, 44.90000000109247225 ) ) ;
#7701 = CARTESIAN_POINT ( 'NONE',  ( -19.41254052147348830, -26.35725562635142083, 18.26367750791695599 ) ) ;
#7702 = DIRECTION ( 'NONE',  ( 0.000000000000000000, 0.000000000000000000, -1.000000000000000000 ) ) ;
#7703 = VECTOR ( 'NONE', #15478, 1000.000000000000000 ) ;
#7704 = CARTESIAN_POINT ( 'NONE',  ( -20.04416526290808065, -25.17491895705300209, 23.73242750791695599 ) ) ;
#7705 = LINE ( 'NONE', #14067, #7164 ) ;
#7706 = DIRECTION ( 'NONE',  ( -0.000000000000000000, -0.7071067811865493491, 0.7071067811865456854 ) ) ;
#7707 = VECTOR ( 'NONE', #14264, 999.9999999999997726 ) ;
#7708 = CARTESIAN_POINT ( 'NONE',  ( -2.066987300000001415, 64.00000000000000000, 46.55000000109247082 ) ) ;
#7709 = CARTESIAN_POINT ( 'NONE',  ( -41.00000000000000711, 53.00000000000000711, -30.99999999999999645 ) ) ;
#7710 = LINE ( 'NONE', #6241, #19147 ) ;
#7711 = DIRECTION ( 'NONE',  ( -1.000000000000000000, 0.000000000000000000, -0.000000000000000000 ) ) ;
#7712 = CARTESIAN_POINT ( 'NONE',  ( -2.066987300000001415, 63.14382582708705627, 46.60000000109246088 ) ) ;
#7713 = CARTESIAN_POINT ( 'NONE',  ( 1.844224359752661968, -41.39960408384398249, 3.000000000000000000 ) ) ;
#7714 = EDGE_CURVE ( 'NONE', #6553, #11839, #13236, .T. ) ;
#7715 = EDGE_CURVE ( 'NONE', #15519, #2028, #17760, .T. ) ;
#7716 = DIRECTION ( 'NONE',  ( -1.942890293094023946E-16, 0.7071067811865456854, 0.7071067811865494601 ) ) ;
#7717 = EDGE_LOOP ( 'NONE', ( #7347, #7026, #14354, #3323 ) ) ;
#7718 = VERTEX_POINT ( 'NONE', #10588 ) ;
#7719 = EDGE_CURVE ( 'NONE', #18999, #5693, #1389, .T. ) ;
#7720 = CARTESIAN_POINT ( 'NONE',  ( -15.16482700510264436, -16.99999999999997868, 21.98632249208304046 ) ) ;
#7721 = VECTOR ( 'NONE', #2958, 1000.000000000000000 ) ;
#7722 =( NAMED_UNIT ( * ) PLANE_ANGLE_UNIT ( ) SI_UNIT ( $, .RADIAN. ) );
#7723 = VECTOR ( 'NONE', #8011, 1000.000000000000000 ) ;
#7724 = CARTESIAN_POINT ( 'NONE',  ( -16.50457296725825174, -19.04416526290807354, 6.017572492083041347 ) ) ;
#7726 = ORIENTED_EDGE ( 'NONE', *, *, #6706, .T. ) ;
#7725 = VERTEX_POINT ( 'NONE', #5898 ) ;
#7727 = CARTESIAN_POINT ( 'NONE',  ( -14.83517299489738761, -20.99999999999997513, 20.01367750791696309 ) ) ;
#7728 = CARTESIAN_POINT ( 'NONE',  ( 1.300000000000000044, 0.000000000000000000, 0.000000000000000000 ) ) ;
#7729 = CARTESIAN_POINT ( 'NONE',  ( -8.044165262908093084, -21.95952864787946979, 12.58007249208304046 ) ) ;
#7730 = CARTESIAN_POINT ( 'NONE',  ( 2.066987300000001415, 64.00000000000000000, 48.35000000109246798 ) ) ;
#7731 = CARTESIAN_POINT ( 'NONE',  ( 1.461580736456473684, 65.46158073645646880, 46.05000000109246372 ) ) ;
#7732 = EDGE_LOOP ( 'NONE', ( #17142, #404, #2840, #10418 ) ) ;
#7733 = EDGE_LOOP ( 'NONE', ( #18432, #5791, #1993, #2105 ) ) ;
#7734 = CARTESIAN_POINT ( 'NONE',  ( -1.530808498934192803E-16, 66.50000000000000000, 45.90000000218494591 ) ) ;
#7735 = DIRECTION ( 'NONE',  ( -0.000000000000000000, 1.000000000000000000, -0.000000000000000000 ) ) ;
#7736 = ORIENTED_EDGE ( 'NONE', *, *, #10424, .T. ) ;
#7737 = CARTESIAN_POINT ( 'NONE',  ( 0.8561741729129460632, 66.06698730000000808, 49.30000000109246372 ) ) ;
#7738 = DIRECTION ( 'NONE',  ( 2.220446049250312834E-16, 0.7071067811865455743, 0.7071067811865493491 ) ) ;
#7739 =( GEOMETRIC_REPRESENTATION_CONTEXT ( 3 ) GLOBAL_UNCERTAINTY_ASSIGNED_CONTEXT ( ( #11195 ) ) GLOBAL_UNIT_ASSIGNED_CONTEXT ( ( #16965, #18138, #1862 ) ) REPRESENTATION_CONTEXT ( 'NONE', 'WORKASPACE' ) );
#7740 = CARTESIAN_POINT ( 'NONE',  ( 3.796994071234847710E-16, 61.93301269999999903, 45.15000000109247225 ) ) ;
#7741 = VECTOR ( 'NONE', #14643, 1000.000000000000000 ) ;
#7742 = EDGE_CURVE ( 'NONE', #15997, #2343, #48, .T. ) ;
#7743 = CARTESIAN_POINT ( 'NONE',  ( -41.00000000000000711, 110.0000000000000000, 27.50000000000000000 ) ) ;
#7744 = DIRECTION ( 'NONE',  ( -1.000000000000000000, 0.000000000000000000, -1.541976423090495633E-16 ) ) ;
#7745 = ORIENTED_EDGE ( 'NONE', *, *, #7145, .T. ) ;
#7747 = VERTEX_POINT ( 'NONE', #7562 ) ;
#7746 = ORIENTED_EDGE ( 'NONE', *, *, #15046, .F. ) ;
#7748 = CARTESIAN_POINT ( 'NONE',  ( -18.35725562635144925, -17.85540867095761186, 14.32617750791695599 ) ) ;
#7749 = ORIENTED_EDGE ( 'NONE', *, *, #7972, .T. ) ;
#7750 = VERTEX_POINT ( 'NONE', #14920 ) ;
#7751 = CARTESIAN_POINT ( 'NONE',  ( -15.63902057219073605, -27.04416526290807710, 14.33007249208304223 ) ) ;
#7752 = CARTESIAN_POINT ( 'NONE',  ( -22.04416526290807710, -25.71081734191525925, 7.982427507916956877 ) ) ;
#7753 = STYLED_ITEM ( 'NONE', ( #17513 ), #1517 ) ;
#7754 = CARTESIAN_POINT ( 'NONE',  ( -2.066987300000001415, 64.00000000000000000, 48.75000000109246656 ) ) ;
#7755 = LINE ( 'NONE', #2843, #928 ) ;
#7756 = ORIENTED_EDGE ( 'NONE', *, *, #7122, .T. ) ;
#7757 = CARTESIAN_POINT ( 'NONE',  ( -14.36097942780923731, -27.04416526290806999, 11.91992750791695954 ) ) ;
#7758 = LINE ( 'NONE', #14015, #2225 ) ;
#7759 = ORIENTED_EDGE ( 'NONE', *, *, #16094, .F. ) ;
#7760 = CARTESIAN_POINT ( 'NONE',  ( -3.065533689247737392, -45.28611686177728046, 3.000000000000000000 ) ) ;
#7761 = EDGE_LOOP ( 'NONE', ( #14913, #11961, #11235, #14606 ) ) ;
#7762 =( LENGTH_UNIT ( ) NAMED_UNIT ( * ) SI_UNIT ( .MILLI., .METRE. ) );
#7763 = CARTESIAN_POINT ( 'NONE',  ( -7.499999999999994671, -38.00000000000000000, 9.500000000000001776 ) ) ;
#7764 = PLANE ( 'NONE',  #7032 ) ;
#7765 = LINE ( 'NONE', #10394, #10670 ) ;
#7766 = CONTEXT_DEPENDENT_SHAPE_REPRESENTATION ( #17709, #6906 ) ;
#7767 = EDGE_CURVE ( 'NONE', #9938, #16368, #11966, .T. ) ;
#7768 = DIRECTION ( 'NONE',  ( -1.000000000000000000, 0.000000000000000000, 0.000000000000000000 ) ) ;
#7769 = CARTESIAN_POINT ( 'NONE',  ( 2.500000000000001776, 64.00000000000000000, 48.10000000218494165 ) ) ;
#7770 = CARTESIAN_POINT ( 'NONE',  ( -10.04416526290807710, -25.50457296725819489, 37.29492750791697375 ) ) ;
#7771 = CARTESIAN_POINT ( 'NONE',  ( -47.00000000000002132, 30.00000000000000000, -60.00000000000002132 ) ) ;
#7772 = ORIENTED_EDGE ( 'NONE', *, *, #3279, .T. ) ;
#7773 = CARTESIAN_POINT ( 'NONE',  ( -19.41254052147348830, -26.35725562635142083, 18.26367750791695599 ) ) ;
#7774 = CARTESIAN_POINT ( 'NONE',  ( -41.00000000000000711, 110.0000000000000000, -38.50000000000000711 ) ) ;
#7775 = ORIENTED_EDGE ( 'NONE', *, *, #15915, .T. ) ;
#7776 = CARTESIAN_POINT ( 'NONE',  ( -12.64274437364858628, -19.58745947852646552, 17.17382249208304401 ) ) ;
#7777 = ADVANCED_FACE ( 'NONE', ( #7363 ), #15013, .F. ) ;
#7778 = CARTESIAN_POINT ( 'NONE',  ( -13.35725562635141195, -26.51566270880198672, 18.92382249208304401 ) ) ;
#7779 = CARTESIAN_POINT ( 'NONE',  ( 43.50000000000001421, 118.0000000000000142, 32.49999999999998579 ) ) ;
#7780 = ORIENTED_EDGE ( 'NONE', *, *, #6402, .F. ) ;
#7781 = CARTESIAN_POINT ( 'NONE',  ( 8.000000000000003553, -32.00000000000000711, 0.000000000000000000 ) ) ;
#7782 = ORIENTED_EDGE ( 'NONE', *, *, #17380, .F. ) ;
#7783 = DIRECTION ( 'NONE',  ( -0.000000000000000000, 0.7071067811865452413, 0.7071067811865497932 ) ) ;
#7784 = LINE ( 'NONE', #13752, #3301 ) ;
#7785 = LINE ( 'NONE', #8950, #16301 ) ;
#7786 = EDGE_CURVE ( 'NONE', #17050, #1646, #1589, .T. ) ;
#7787 = DIRECTION ( 'NONE',  ( 0.000000000000000000, -0.7071067811865495711, 0.7071067811865454633 ) ) ;
#7788 = DIRECTION ( 'NONE',  ( -1.000000000000000000, 0.000000000000000000, 0.000000000000000000 ) ) ;
#7789 = FACE_OUTER_BOUND ( 'NONE', #5290, .T. ) ;
#7790 = LINE ( 'NONE', #12762, #2684 ) ;
#7791 = ORIENTED_EDGE ( 'NONE', *, *, #4978, .T. ) ;
#7792 = VECTOR ( 'NONE', #18687, 1000.000000000000000 ) ;
#7793 = CARTESIAN_POINT ( 'NONE',  ( 65.00000000000000000, 0.000000000000000000, 0.000000000000000000 ) ) ;
#7794 = CARTESIAN_POINT ( 'NONE',  ( -10.04416526290807710, -25.50457296725819489, 16.29492750791695954 ) ) ;
#7795 = CARTESIAN_POINT ( 'NONE',  ( 1.767766952966370653, 62.23223304703363112, 45.60000000218494165 ) ) ;
#7796 = CARTESIAN_POINT ( 'NONE',  ( -9.999999999999994671, -23.83517299489734143, 18.04882249208304401 ) ) ;
#7797 = DIRECTION ( 'NONE',  ( 0.000000000000000000, 0.000000000000000000, -1.000000000000000000 ) ) ;
#7798 = CARTESIAN_POINT ( 'NONE',  ( -16.17491895705301275, -18.95583473709189803, 14.54492750791695421 ) ) ;
#7799 = LINE ( 'NONE', #16423, #4861 ) ;
#7801 = CARTESIAN_POINT ( 'NONE',  ( -20.04416526290808065, -25.17491895705300209, 18.48242750791695599 ) ) ;
#7800 = AXIS2_PLACEMENT_3D ( 'NONE', #10263, #7534, #1462 ) ;
#7802 = DIRECTION ( 'NONE',  ( 0.000000000000000000, 0.000000000000000000, -1.000000000000000000 ) ) ;
#7803 = LINE ( 'NONE', #7239, #10693 ) ;
#7804 = CARTESIAN_POINT ( 'NONE',  ( -2.066987300000001415, 63.14382582708705627, 49.00000000109246656 ) ) ;
#7805 = CARTESIAN_POINT ( 'NONE',  ( 44.99999999999997158, -1.285879139104706187E-16, 56.59999999999999432 ) ) ;
#7806 = AXIS2_PLACEMENT_3D ( 'NONE', #9461, #13970, #543 ) ;
#7807 = CARTESIAN_POINT ( 'NONE',  ( -50.00000000000002132, 118.0000000000000142, 40.49999999999997868 ) ) ;
#7808 = PLANE ( 'NONE',  #5226 ) ;
#7809 = CARTESIAN_POINT ( 'NONE',  ( 1.461580736456473906, 62.53841926354353120, 48.45000000109246940 ) ) ;
#7810 = EDGE_CURVE ( 'NONE', #9430, #15274, #17861, .T. ) ;
#7811 = EDGE_CURVE ( 'NONE', #10184, #8734, #13429, .T. ) ;
#7812 = LINE ( 'NONE', #6442, #18966 ) ;
#7813 = ORIENTED_EDGE ( 'NONE', *, *, #3571, .F. ) ;
#7814 = ORIENTED_EDGE ( 'NONE', *, *, #6055, .T. ) ;
#7815 = CARTESIAN_POINT ( 'NONE',  ( -21.95583473709189803, -26.04047135212049469, 25.70507249208304046 ) ) ;
#7816 = EDGE_CURVE ( 'NONE', #535, #8383, #7662, .T. ) ;
#7817 = AXIS2_PLACEMENT_3D ( 'NONE', #7478, #17881, #35 ) ;
#7818 = PRESENTATION_STYLE_ASSIGNMENT (( #18411 ) ) ;
#7819 = CARTESIAN_POINT ( 'NONE',  ( -10.04416526290808598, -22.49542703274172695, 7.330072492083041347 ) ) ;
#7820 = EDGE_LOOP ( 'NONE', ( #17242, #4026, #8172, #3271 ) ) ;
#7821 = CARTESIAN_POINT ( 'NONE',  ( -17.99999999999999645, -23.83517299489736985, 13.45117750791696309 ) ) ;
#7822 = DIRECTION ( 'NONE',  ( -1.000000000000000000, 0.000000000000000000, -0.000000000000000000 ) ) ;
#7823 = CARTESIAN_POINT ( 'NONE',  ( -8.855408670957602979, -27.35725562635137820, 18.48632249208304046 ) ) ;
#7824 = AXIS2_PLACEMENT_3D ( 'NONE', #12301, #18296, #17675 ) ;
#7825 = AXIS2_PLACEMENT_3D ( 'NONE', #12429, #15569, #8225 ) ;
#7826 = CARTESIAN_POINT ( 'NONE',  ( 32.50000000000000000, -6.000000000000000000, -42.49999999999999289 ) ) ;
#7827 = CARTESIAN_POINT ( 'NONE',  ( -1.461580736456473906, 65.46158073645646880, 47.85000000109246798 ) ) ;
#7828 = VERTEX_POINT ( 'NONE', #4434 ) ;
#7829 = ORIENTED_EDGE ( 'NONE', *, *, #1701, .F. ) ;
#7830 = DIRECTION ( 'NONE',  ( 0.000000000000000000, 0.000000000000000000, -1.000000000000000000 ) ) ;
#7831 = CARTESIAN_POINT ( 'NONE',  ( -41.00000000000000711, 110.0000000000000000, -19.00000000000000000 ) ) ;
#7832 = EDGE_CURVE ( 'NONE', #1050, #15591, #7765, .T. ) ;
#7833 = AXIS2_PLACEMENT_3D ( 'NONE', #3277, #527, #12475 ) ;
#7834 = EDGE_LOOP ( 'NONE', ( #18789, #6273, #17012, #4905 ) ) ;
#7835 = CARTESIAN_POINT ( 'NONE',  ( -2.500000000000001776, 64.00000000000000000, 46.79999999999999716 ) ) ;
#7836 = DIRECTION ( 'NONE',  ( 1.000000000000000000, 0.000000000000000000, 0.000000000000000000 ) ) ;
#7837 = ADVANCED_FACE ( 'NONE', ( #12158 ), #16387, .F. ) ;
#7838 = EDGE_CURVE ( 'NONE', #11652, #7898, #9129, .T. ) ;
#7839 = AXIS2_PLACEMENT_3D ( 'NONE', #9904, #806, #11371 ) ;
#7840 = PLANE ( 'NONE',  #15392 ) ;
#7841 = CARTESIAN_POINT ( 'NONE',  ( 34.99999999999999289, 0.000000000000000000, 42.49999999999997868 ) ) ;
#7842 = VECTOR ( 'NONE', #13007, 1000.000000000000000 ) ;
#7843 = CARTESIAN_POINT ( 'NONE',  ( -1.767766952966369765, 62.23223304703363112, 45.40000000218494591 ) ) ;
#7844 = VERTEX_POINT ( 'NONE', #215 ) ;
#7846 = ORIENTED_EDGE ( 'NONE', *, *, #10910, .F. ) ;
#7845 = ORIENTED_EDGE ( 'NONE', *, *, #3754, .F. ) ;
#7847 = CARTESIAN_POINT ( 'NONE',  ( -18.64274437364853654, -29.97976432393976509, 28.32617750791695954 ) ) ;
#7848 = ORIENTED_EDGE ( 'NONE', *, *, #4655, .T. ) ;
#7849 = STYLED_ITEM ( 'NONE', ( #5314 ), #3741 ) ;
#7850 = ORIENTED_EDGE ( 'NONE', *, *, #3682, .F. ) ;
#7851 = CARTESIAN_POINT ( 'NONE',  ( -16.64274437364858272, -21.48433729119797420, 11.04882249208304223 ) ) ;
#7852 = CARTESIAN_POINT ( 'NONE',  ( -22.04416526290807710, -25.71081734191525925, 18.48242750791695954 ) ) ;
#7853 = CARTESIAN_POINT ( 'NONE',  ( 3.796994071234847710E-16, 61.93301269999999903, 47.35000000109246798 ) ) ;
#7854 = CARTESIAN_POINT ( 'NONE',  ( -25.00000000000000711, 53.00000000000000711, -18.00000000000000000 ) ) ;
#7855 = ORIENTED_EDGE ( 'NONE', *, *, #965, .F. ) ;
#7856 = CARTESIAN_POINT ( 'NONE',  ( -12.68318583509884157, -21.92450931948787485, 10.16992750791695954 ) ) ;
#7857 = VECTOR ( 'NONE', #787, 1000.000000000000000 ) ;
#7858 =( LENGTH_UNIT ( ) NAMED_UNIT ( * ) SI_UNIT ( .MILLI., .METRE. ) );
#7859 = ORIENTED_EDGE ( 'NONE', *, *, #10439, .F. ) ;
#7860 = EDGE_CURVE ( 'NONE', #17638, #11652, #14, .T. ) ;
#7861 = EDGE_CURVE ( 'NONE', #10544, #109, #15115, .T. ) ;
#7862 = CARTESIAN_POINT ( 'NONE',  ( 4.999999999999997335, 3.306546357697854226E-16, 2.700000000000000622 ) ) ;
#7863 = VERTEX_POINT ( 'NONE', #9223 ) ;
#7864 = CARTESIAN_POINT ( 'NONE',  ( 1.300000000000000044, 0.000000000000000000, 0.000000000000000000 ) ) ;
#7865 = FACE_OUTER_BOUND ( 'NONE', #10697, .T. ) ;
#7866 = DIRECTION ( 'NONE',  ( -1.000000000000000000, 0.000000000000000000, 0.000000000000000000 ) ) ;
#7867 = CARTESIAN_POINT ( 'NONE',  ( -2.066987300000001415, 64.00000000000000000, 48.75000000109246656 ) ) ;
#7868 = CONTEXT_DEPENDENT_SHAPE_REPRESENTATION ( #15461, #16483 ) ;
#7869 = EDGE_CURVE ( 'NONE', #2736, #4857, #18157, .T. ) ;
#7870 = CARTESIAN_POINT ( 'NONE',  ( -2.500000000000001776, 65.03553390593273775, 49.25000000218494023 ) ) ;
#7871 = DIRECTION ( 'NONE',  ( -1.000000000000000000, 0.000000000000000000, 0.000000000000000000 ) ) ;
#7872 = VECTOR ( 'NONE', #14617, 1000.000000000000000 ) ;
#7873 = DIRECTION ( 'NONE',  ( -1.000000000000000000, 0.000000000000000000, 0.000000000000000000 ) ) ;
#7874 = CARTESIAN_POINT ( 'NONE',  ( 2.500000000000000000, 1.178949249685212974, -2.042000000000001148 ) ) ;
#7875 = ORIENTED_EDGE ( 'NONE', *, *, #36, .T. ) ;
#7876 = CARTESIAN_POINT ( 'NONE',  ( -12.35725562635143682, -19.75228648362908501, 20.45117750791695954 ) ) ;
#7877 = AXIS2_PLACEMENT_3D ( 'NONE', #17414, #11512, #6929 ) ;
#7878 = DIRECTION ( 'NONE',  ( -1.000000000000000000, 0.000000000000000000, -0.000000000000000000 ) ) ;
#7879 = ORIENTED_EDGE ( 'NONE', *, *, #3495, .F. ) ;
#7880 = CARTESIAN_POINT ( 'NONE',  ( -18.78091578003892081, -20.46040770435013556, 16.08007249208304401 ) ) ;
#7881 = EDGE_CURVE ( 'NONE', #16382, #8256, #1784, .T. ) ;
#7882 = CARTESIAN_POINT ( 'NONE',  ( -13.64274437364857739, -21.31951028609534760, 17.17382249208304401 ) ) ;
#7883 = LINE ( 'NONE', #425, #7210 ) ;
#7884 = EDGE_LOOP ( 'NONE', ( #573, #14627, #2513, #17197, #14828, #13816, #7428, #3747 ) ) ;
#7885 = VECTOR ( 'NONE', #9906, 1000.000000000000000 ) ;
#7886 = CARTESIAN_POINT ( 'NONE',  ( -45.00000000000000000, 3.000000000000000000, 56.49999999999998579 ) ) ;
#7887 = ORIENTED_EDGE ( 'NONE', *, *, #8436, .T. ) ;
#7888 = LINE ( 'NONE', #12380, #12196 ) ;
#7889 = DIRECTION ( 'NONE',  ( 0.000000000000000000, 0.000000000000000000, -1.000000000000000000 ) ) ;
#7890 = VECTOR ( 'NONE', #3439, 1000.000000000000000 ) ;
#7891 = CARTESIAN_POINT ( 'NONE',  ( -41.00000000000000711, 53.00000000000000711, -5.000000000000000888 ) ) ;
#7892 = CARTESIAN_POINT ( 'NONE',  ( -41.00000000000000711, 53.00000000000000711, -37.50000000000000711 ) ) ;
#7893 = VECTOR ( 'NONE', #8121, 1000.000000000000000 ) ;
#7894 =( NAMED_UNIT ( * ) PLANE_ANGLE_UNIT ( ) SI_UNIT ( $, .RADIAN. ) );
#7895 = FACE_BOUND ( 'NONE', #8405, .T. ) ;
#7896 = DIRECTION ( 'NONE',  ( 0.000000000000000000, -1.000000000000000000, 0.000000000000000000 ) ) ;
#7897 = AXIS2_PLACEMENT_3D ( 'NONE', #15256, #12106, #14072 ) ;
#7898 = VERTEX_POINT ( 'NONE', #10289 ) ;
#7899 = AXIS2_PLACEMENT_3D ( 'NONE', #12103, #12306, #16825 ) ;
#7900 = CARTESIAN_POINT ( 'NONE',  ( 44.99999999999998579, -3.000000000000002665, -54.99999999999998579 ) ) ;
#7901 = CARTESIAN_POINT ( 'NONE',  ( -9.955834737091912245, -22.82508104294696594, 15.85742750791695777 ) ) ;
#7902 = CARTESIAN_POINT ( 'NONE',  ( 2.500000000000002220, 62.96446609406726935, 47.25000000218494023 ) ) ;
#7903 = CARTESIAN_POINT ( 'NONE',  ( -19.41254052147350961, -21.64274437364857562, 15.86132249208304223 ) ) ;
#7904 = DIRECTION ( 'NONE',  ( 0.000000000000000000, -1.000000000000000000, 0.000000000000000000 ) ) ;
#7905 = CARTESIAN_POINT ( 'NONE',  ( -13.82508104294698192, -29.04416526290806644, 11.91992750791695421 ) ) ;
#7906 = CARTESIAN_POINT ( 'NONE',  ( -7.999999999999986677, 60.00000000000000711, 45.00000000000000000 ) ) ;
#7907 = CARTESIAN_POINT ( 'NONE',  ( -10.58745947852649927, -21.64274437364853654, 20.88867750791695954 ) ) ;
#7908 = LINE ( 'NONE', #12400, #3730 ) ;
#7909 = CARTESIAN_POINT ( 'NONE',  ( -2.750000000000020872, 118.0000000000000142, 40.49999999999995737 ) ) ;
#7910 = CARTESIAN_POINT ( 'NONE',  ( -0.8561741729129465073, 61.93301270000000613, 47.50000000109246656 ) ) ;
#7911 = LINE ( 'NONE', #1826, #8711 ) ;
#7912 = SHAPE_REPRESENTATION ( 'BR-818', ( #10799, #17375, #19262, #15504, #8598, #4873, #2036, #13932, #7031, #7994, #6111, #5470, #788, #1088, #9849, #18938, #4545, #3917, #2652, #158 ), #12374 ) ;
#7913 = VECTOR ( 'NONE', #4962, 1000.000000000000000 ) ;
#7914 = CARTESIAN_POINT ( 'NONE',  ( 0.000000000000000000, 64.00000000000000000, 49.99999999999999289 ) ) ;
#7915 = FACE_OUTER_BOUND ( 'NONE', #12080, .T. ) ;
#7916 = CARTESIAN_POINT ( 'NONE',  ( 2.066987300000001859, 64.85617417291294373, 49.40000000109246514 ) ) ;
#7917 = FACE_OUTER_BOUND ( 'NONE', #1015, .T. ) ;
#7918 = ORIENTED_EDGE ( 'NONE', *, *, #8373, .T. ) ;
#7919 = EDGE_LOOP ( 'NONE', ( #224, #181, #5453, #18333 ) ) ;
#7920 = CARTESIAN_POINT ( 'NONE',  ( -20.97976432393974022, -27.64274437364858628, 30.73632249208304046 ) ) ;
#7921 =( LENGTH_UNIT ( ) NAMED_UNIT ( * ) SI_UNIT ( .MILLI., .METRE. ) );
#7922 = CARTESIAN_POINT ( 'NONE',  ( -18.53959229564983247, -27.78091578003891016, 14.76757249208303868 ) ) ;
#7923 = ORIENTED_EDGE ( 'NONE', *, *, #476, .T. ) ;
#7924 = CARTESIAN_POINT ( 'NONE',  ( -17.51566270880201159, -22.35725562635141728, 29.63867750791695954 ) ) ;
#7925 = DIRECTION ( 'NONE',  ( 1.000000000000000000, 0.000000000000000000, 9.251858538542970348E-17 ) ) ;
#7926 = CARTESIAN_POINT ( 'NONE',  ( -21.99999999999999289, -24.16482700510262305, 15.42382249208304046 ) ) ;
#7927 = CARTESIAN_POINT ( 'NONE',  ( -2.066987300000001415, 64.00000000000000000, 47.95000000109246940 ) ) ;
#7928 = CARTESIAN_POINT ( 'NONE',  ( 1.461580736456473906, 62.53841926354353120, 45.05000000109246372 ) ) ;
#7929 = ORIENTED_EDGE ( 'NONE', *, *, #15942, .T. ) ;
#7930 = ORIENTED_EDGE ( 'NONE', *, *, #6435, .F. ) ;
#7931 = ADVANCED_FACE ( 'NONE', ( #2854 ), #8835, .T. ) ;
#7932 = EDGE_CURVE ( 'NONE', #9301, #13286, #503, .T. ) ;
#7933 = DIRECTION ( 'NONE',  ( 1.000000000000000000, -0.000000000000000000, -0.000000000000000000 ) ) ;
#7934 = CARTESIAN_POINT ( 'NONE',  ( -37.50000000000002132, 107.3545527679194436, 24.99999999999998224 ) ) ;
#7935 = DIRECTION ( 'NONE',  ( -0.7071067811865486830, -0.5000000000000005551, 0.4999999999999978351 ) ) ;
#7936 = CARTESIAN_POINT ( 'NONE',  ( -10.00000000000000000, 0.000000000000000000, -3.000000000000000000 ) ) ;
#7937 = EDGE_CURVE ( 'NONE', #19283, #13814, #9513, .T. ) ;
#7938 = CARTESIAN_POINT ( 'NONE',  ( -0.8561741729129461742, 66.06698729999999387, 44.80000000109246372 ) ) ;
#7939 = DIRECTION ( 'NONE',  ( 1.000000000000000000, 0.000000000000000000, 0.000000000000000000 ) ) ;
#7940 = EDGE_CURVE ( 'NONE', #9239, #14297, #1882, .T. ) ;
#7941 = DIRECTION ( 'NONE',  ( 0.000000000000000000, 0.000000000000000000, 1.000000000000000000 ) ) ;
#7942 = ORIENTED_EDGE ( 'NONE', *, *, #11656, .T. ) ;
#7944 = VERTEX_POINT ( 'NONE', #3445 ) ;
#7943 = VERTEX_POINT ( 'NONE', #10780 ) ;
#7945 = CARTESIAN_POINT ( 'NONE',  ( -18.64274437364853654, -29.97976432393976509, 33.57617750791695954 ) ) ;
#7946 = ORIENTED_EDGE ( 'NONE', *, *, #4704, .F. ) ;
#7947 = ORIENTED_EDGE ( 'NONE', *, *, #11613, .F. ) ;
#7948 = CARTESIAN_POINT ( 'NONE',  ( -17.95583473709190869, -24.96867458239598037, 36.20507249208304756 ) ) ;
#7949 = CARTESIAN_POINT ( 'NONE',  ( -21.14459132904236327, -27.35725562635143149, 18.26367750791695599 ) ) ;
#7950 = CARTESIAN_POINT ( 'NONE',  ( -1.265664690411616068E-16, 66.06698730000000808, 47.75000000109246656 ) ) ;
#7951 = DIRECTION ( 'NONE',  ( 1.000000000000000000, 0.000000000000000000, 0.000000000000000000 ) ) ;
#7952 = ORIENTED_EDGE ( 'NONE', *, *, #8308, .T. ) ;
#7953 = CARTESIAN_POINT ( 'NONE',  ( -14.03132541760401786, -21.04416526290806289, 9.732427507916959541 ) ) ;
#7954 = ADVANCED_FACE ( 'NONE', ( #18451 ), #4124, .F. ) ;
#7955 = VERTEX_POINT ( 'NONE', #13898 ) ;
#7956 = DIRECTION ( 'NONE',  ( -0.000000000000000000, -0.000000000000000000, -1.000000000000000000 ) ) ;
#7957 = ORIENTED_EDGE ( 'NONE', *, *, #887, .T. ) ;
#7958 = CARTESIAN_POINT ( 'NONE',  ( 0.1249999999999895917, 25.46464466094064250, 60.66708332270462734 ) ) ;
#7959 = PLANE ( 'NONE',  #13155 ) ;
#7960 = PLANE ( 'NONE',  #14720 ) ;
#7961 = DIRECTION ( 'NONE',  ( 0.000000000000000000, 0.000000000000000000, 1.000000000000000000 ) ) ;
#7962 = CARTESIAN_POINT ( 'NONE',  ( 44.99999999999998579, 3.000000000000000000, -54.99999999999998579 ) ) ;
#7963 = CARTESIAN_POINT ( 'NONE',  ( 1.461580736456473684, 65.46158073645646880, 48.45000000109247651 ) ) ;
#7964 = CONTEXT_DEPENDENT_SHAPE_REPRESENTATION ( #435, #10354 ) ;
#7965 = CARTESIAN_POINT ( 'NONE',  ( -50.00000000000001421, 0.000000000000000000, 59.99999999999997868 ) ) ;
#7966 = LINE ( 'NONE', #598, #7536 ) ;
#7967 = CARTESIAN_POINT ( 'NONE',  ( -32.50000000000000000, 53.00000000000000711, 15.00000000000000000 ) ) ;
#7968 = FACE_OUTER_BOUND ( 'NONE', #426, .T. ) ;
#7969 = ORIENTED_EDGE ( 'NONE', *, *, #16089, .F. ) ;
#7970 = CARTESIAN_POINT ( 'NONE',  ( -19.99999999999999645, -23.83517299489738051, 34.45117750791696665 ) ) ;
#7971 = DIRECTION ( 'NONE',  ( 0.000000000000000000, 0.000000000000000000, -1.000000000000000000 ) ) ;
#7972 = EDGE_CURVE ( 'NONE', #2146, #12847, #3326, .T. ) ;
#7973 = VERTEX_POINT ( 'NONE', #1849 ) ;
#7974 = ADVANCED_FACE ( 'NONE', ( #18427 ), #7840, .T. ) ;
#7975 = CARTESIAN_POINT ( 'NONE',  ( -9.999999999999994671, -23.83517299489734143, 33.79882249208304046 ) ) ;
#7976 = EDGE_CURVE ( 'NONE', #15072, #9572, #568, .T. ) ;
#7977 = CARTESIAN_POINT ( 'NONE',  ( -17.07549068051208963, -26.31681416490115311, 14.76757249208304223 ) ) ;
#7978 = DIRECTION ( 'NONE',  ( 0.000000000000000000, 0.000000000000000000, -1.000000000000000000 ) ) ;
#7979 = ORIENTED_EDGE ( 'NONE', *, *, #6184, .F. ) ;
#7980 = CARTESIAN_POINT ( 'NONE',  ( -2.066987300000001415, 64.00000000000000000, 49.65000000109247225 ) ) ;
#7981 = EDGE_LOOP ( 'NONE', ( #796, #18636, #7923, #11233, #12336, #3221, #5752 ) ) ;
#7982 = CARTESIAN_POINT ( 'NONE',  ( -40.00000000000000711, 113.0000000000000000, -37.50000000000000711 ) ) ;
#7983 = CARTESIAN_POINT ( 'NONE',  ( -1.767766952966369765, 62.23223304703363112, 46.09999999999999432 ) ) ;
#7984 = MECHANICAL_DESIGN_GEOMETRIC_PRESENTATION_REPRESENTATION (  '', ( #13598 ), #6100 ) ;
#7985 = DIRECTION ( 'NONE',  ( 1.000000000000000000, -0.000000000000000000, -0.000000000000000000 ) ) ;
#7986 = VECTOR ( 'NONE', #1212, 1000.000000000000000 ) ;
#7987 = DIRECTION ( 'NONE',  ( 0.1648270051026194671, 0.000000000000000000, -0.9863224920830413467 ) ) ;
#7988 = EDGE_CURVE ( 'NONE', #9541, #856, #281, .T. ) ;
#7989 = FACE_OUTER_BOUND ( 'NONE', #10086, .T. ) ;
#7990 = ADVANCED_FACE ( 'NONE', ( #9487 ), #12332, .T. ) ;
#7991 = SURFACE_STYLE_FILL_AREA ( #13860 ) ;
#7992 = LINE ( 'NONE', #6703, #6465 ) ;
#7993 = EDGE_LOOP ( 'NONE', ( #17398, #7879, #17509, #14314 ) ) ;
#7994 = AXIS2_PLACEMENT_3D ( 'NONE', #4661, #17988, #1813 ) ;
#7995 = CARTESIAN_POINT ( 'NONE',  ( -18.53959229564986799, -20.21908421996107563, 19.35742750791695599 ) ) ;
#7996 = VECTOR ( 'NONE', #2012, 1000.000000000000000 ) ;
#7997 = CARTESIAN_POINT ( 'NONE',  ( -2.500000000000000888, 62.96446609406726935, 46.95000000218495018 ) ) ;
#7998 = CARTESIAN_POINT ( 'NONE',  ( -11.21908421996106320, -27.53959229564982181, 18.70507249208304401 ) ) ;
#7999 = LINE ( 'NONE', #13965, #18240 ) ;
#8000 = CARTESIAN_POINT ( 'NONE',  ( -13.49542703274178379, -19.04416526290806289, 9.732427507916959541 ) ) ;
#8001 = CARTESIAN_POINT ( 'NONE',  ( -31.74999999999995737, 0.000000000000000000, 0.000000000000000000 ) ) ;
#8002 = CARTESIAN_POINT ( 'NONE',  ( -13.82508104294698015, -29.04416526290806289, 11.91992750791695777 ) ) ;
#8003 = CARTESIAN_POINT ( 'NONE',  ( -1.035533905932738863, 61.50000000000000000, 46.95000000000000284 ) ) ;
#8004 = CARTESIAN_POINT ( 'NONE',  ( -10.75228648362912232, -21.35725562635138530, 28.11132249208304046 ) ) ;
#8005 = CARTESIAN_POINT ( 'NONE',  ( -2.066987300000001415, 64.00000000000000000, 47.35000000109246798 ) ) ;
#8006 = DIRECTION ( 'NONE',  ( -0.000000000000000000, -0.000000000000000000, -1.000000000000000000 ) ) ;
#8007 = VECTOR ( 'NONE', #10372, 1000.000000000000000 ) ;
#8008 = LINE ( 'NONE', #13976, #6635 ) ;
#8009 = VECTOR ( 'NONE', #14237, 1000.000000000000000 ) ;
#8010 = ADVANCED_FACE ( 'NONE', ( #12526 ), #5094, .F. ) ;
#8011 = DIRECTION ( 'NONE',  ( 0.000000000000000000, 1.000000000000000000, 0.000000000000000000 ) ) ;
#8012 = CARTESIAN_POINT ( 'NONE',  ( -2.066987300000001415, 64.00000000000000000, 48.95000000109246940 ) ) ;
#8013 = DIRECTION ( 'NONE',  ( 0.000000000000000000, 0.000000000000000000, -1.000000000000000000 ) ) ;
#8014 = EDGE_LOOP ( 'NONE', ( #14327, #401, #14938, #5524 ) ) ;
#8015 = VERTEX_POINT ( 'NONE', #3608 ) ;
#8016 = CARTESIAN_POINT ( 'NONE',  ( -9.996306089212408708, -18.75498260482328661, 33.14257249208303335 ) ) ;
#8017 = SURFACE_STYLE_FILL_AREA ( #10742 ) ;
#8018 = CARTESIAN_POINT ( 'NONE',  ( -13.49542703274174116, -28.95583473709188738, 8.642572492083040459 ) ) ;
#8019 = EDGE_LOOP ( 'NONE', ( #4906, #11626, #440, #18176 ) ) ;
#8020 = CARTESIAN_POINT ( 'NONE',  ( -17.31681416490115311, -26.07549068051209318, 28.54492750791696665 ) ) ;
#8021 = LINE ( 'NONE', #4983, #8024 ) ;
#8022 = CARTESIAN_POINT ( 'NONE',  ( -9.754982604823302594, -29.00369391078756465, 13.45507249208303868 ) ) ;
#8023 = AXIS2_PLACEMENT_3D ( 'NONE', #17938, #10267, #17540 ) ;
#8024 = VECTOR ( 'NONE', #9373, 1000.000000000000000 ) ;
#8025 = CARTESIAN_POINT ( 'NONE',  ( 1.461580736456473906, 62.53841926354353120, 47.45000000109246940 ) ) ;
#8026 = CARTESIAN_POINT ( 'NONE',  ( 2.066987300000002303, 63.14382582708705627, 46.70000000109248361 ) ) ;
#8027 = ORIENTED_EDGE ( 'NONE', *, *, #5333, .F. ) ;
#8028 = ORIENTED_EDGE ( 'NONE', *, *, #8229, .T. ) ;
#8029 = FACE_OUTER_BOUND ( 'NONE', #4267, .T. ) ;
#8030 = DIRECTION ( 'NONE',  ( -1.000000000000000000, 0.000000000000000000, 0.000000000000000000 ) ) ;
#8031 = CARTESIAN_POINT ( 'NONE',  ( 3.796994071234847710E-16, 61.93301269999999903, 48.15000000109247225 ) ) ;
#8032 = PLANE ( 'NONE',  #11543 ) ;
#8033 = CARTESIAN_POINT ( 'NONE',  ( -2.066987300000001859, 64.85617417291294373, 44.90000000109247225 ) ) ;
#8034 = ADVANCED_FACE ( 'NONE', ( #6267 ), #15188, .F. ) ;
#8035 = EDGE_CURVE ( 'NONE', #10686, #6595, #8124, .T. ) ;
#8036 = LINE ( 'NONE', #11051, #5356 ) ;
#8037 = CIRCLE ( 'NONE', #515, 6.799999999999999822 ) ;
#8038 = VECTOR ( 'NONE', #8478, 1000.000000000000000 ) ;
#8039 = CARTESIAN_POINT ( 'NONE',  ( 32.50000000000000000, -6.000000000000000000, -45.00000000000000000 ) ) ;
#8040 = EDGE_LOOP ( 'NONE', ( #17449, #18055, #1995, #3806 ) ) ;
#8041 = ORIENTED_EDGE ( 'NONE', *, *, #4222, .F. ) ;
#8042 = CARTESIAN_POINT ( 'NONE',  ( -17.04047135212043784, -30.95583473709190159, 28.10742750791695954 ) ) ;
#8043 = DIRECTION ( 'NONE',  ( 0.000000000000000000, 1.000000000000000000, 0.000000000000000000 ) ) ;
#8044 = VERTEX_POINT ( 'NONE', #1756 ) ;
#8045 = VERTEX_POINT ( 'NONE', #12236 ) ;
#8046 = CARTESIAN_POINT ( 'NONE',  ( -16.64274437364858272, -21.48433729119797420, 37.29882249208304046 ) ) ;
#8047 = CARTESIAN_POINT ( 'NONE',  ( -16.71081734191527346, -16.95583473709190159, 19.79492750791695954 ) ) ;
#8048 = CARTESIAN_POINT ( 'NONE',  ( 5.800448907431066559, 29.68308948419212712, 56.80092238452526487 ) ) ;
#8049 = CARTESIAN_POINT ( 'NONE',  ( -37.50000000000002132, 107.3545527679194436, -25.00000000000002132 ) ) ;
#8050 = DIRECTION ( 'NONE',  ( -1.000000000000000000, 0.000000000000000000, 0.000000000000000000 ) ) ;
#8051 = VERTEX_POINT ( 'NONE', #12619 ) ;
#8052 = CARTESIAN_POINT ( 'NONE',  ( -16.35725562635142794, -21.31951028609535470, 30.07617750791696309 ) ) ;
#8053 = VECTOR ( 'NONE', #1172, 1000.000000000000000 ) ;
#8054 = ORIENTED_EDGE ( 'NONE', *, *, #15942, .F. ) ;
#8055 = AXIS2_PLACEMENT_3D ( 'NONE', #18453, #5023, #10983 ) ;
#8056 = CARTESIAN_POINT ( 'NONE',  ( -41.00000000000000711, 53.00000000000000711, -32.00000000000000000 ) ) ;
#8057 = VERTEX_POINT ( 'NONE', #18615 ) ;
#8058 = CARTESIAN_POINT ( 'NONE',  ( 0.000000000000000000, -0.7390083445627200209, 1.280000000000001137 ) ) ;
#8059 = FACE_BOUND ( 'NONE', #4418, .T. ) ;
#8060 = CARTESIAN_POINT ( 'NONE',  ( -21.50000000000000000, 118.0000000000000142, 32.50000000000000000 ) ) ;
#8061 = ADVANCED_FACE ( 'NONE', ( #17323 ), #12709, .F. ) ;
#8062 = DIRECTION ( 'NONE',  ( 1.000000000000000000, -0.000000000000000000, -0.000000000000000000 ) ) ;
#8063 = CARTESIAN_POINT ( 'NONE',  ( -1.461580736456473906, 65.46158073645646880, 49.45000000109246940 ) ) ;
#8064 = ITEM_DEFINED_TRANSFORMATION ( 'NONE', 'NONE', #8598,  #1791 ) ;
#8065 = DIRECTION ( 'NONE',  ( 2.775557561562890858E-16, 0.7071067811865454633, 0.7071067811865496822 ) ) ;
#8066 = FACE_OUTER_BOUND ( 'NONE', #14979, .T. ) ;
#8067 = CARTESIAN_POINT ( 'NONE',  ( -4.101219330881938241, 32.64264068711930378, 53.84264068711927109 ) ) ;
#8068 = CARTESIAN_POINT ( 'NONE',  ( 1.993043451197827665, 65.46727981049029665, 44.99999999999998579 ) ) ;
#8069 = EDGE_LOOP ( 'NONE', ( #16655, #13413, #8709, #3146 ) ) ;
#8070 = EDGE_CURVE ( 'NONE', #9848, #2631, #17413, .T. ) ;
#8071 = CARTESIAN_POINT ( 'NONE',  ( -16.50457296725820555, -28.95583473709189448, 28.10742750791695954 ) ) ;
#8072 = DIRECTION ( 'NONE',  ( -1.000000000000000000, 0.000000000000000000, 0.000000000000000000 ) ) ;
#8073 = VERTEX_POINT ( 'NONE', #3887 ) ;
#8074 = CARTESIAN_POINT ( 'NONE',  ( -16.50457296725825174, -19.04416526290807354, 37.51757249208304046 ) ) ;
#8075 = CARTESIAN_POINT ( 'NONE',  ( -12.31951028609536536, -25.35725562635139596, 34.23632249208304756 ) ) ;
#8076 = DIRECTION ( 'NONE',  ( -1.000000000000000000, 0.000000000000000000, -0.000000000000000000 ) ) ;
#8077 = EDGE_LOOP ( 'NONE', ( #766, #13197, #11001, #14486 ) ) ;
#8078 = DIRECTION ( 'NONE',  ( -0.000000000000000000, 1.000000000000000000, 1.224646799147353207E-16 ) ) ;
#8079 = EDGE_LOOP ( 'NONE', ( #7121, #16567, #4547, #13033 ) ) ;
#8080 = DIRECTION ( 'NONE',  ( 0.000000000000000000, -1.000000000000000000, 0.000000000000000000 ) ) ;
#8081 = DIRECTION ( 'NONE',  ( -0.000000000000000000, -0.000000000000000000, -1.000000000000000000 ) ) ;
#8082 = CARTESIAN_POINT ( 'NONE',  ( -41.00000000000000711, 53.00000000000000711, -6.000000000000001776 ) ) ;
#8083 = ADVANCED_FACE ( 'NONE', ( #18986 ), #11419, .F. ) ;
#8084 = CARTESIAN_POINT ( 'NONE',  ( 4.999999999999993783, 68.00000000000000000, 69.99999999999998579 ) ) ;
#8085 = ADVANCED_FACE ( 'NONE', ( #944 ), #8494, .F. ) ;
#8086 = CARTESIAN_POINT ( 'NONE',  ( -41.00000000000000711, 113.0000000000000000, 30.00000000000000000 ) ) ;
#8087 =( REPRESENTATION_RELATIONSHIP ('NONE','NONE', #7912, #7269 ) REPRESENTATION_RELATIONSHIP_WITH_TRANSFORMATION ( #9419 )SHAPE_REPRESENTATION_RELATIONSHIP( ) );
#8088 = FACE_OUTER_BOUND ( 'NONE', #7328, .T. ) ;
#8089 = CARTESIAN_POINT ( 'NONE',  ( -40.00000000000000711, 113.0000000000000000, -38.50000000000000711 ) ) ;
#8090 = VERTEX_POINT ( 'NONE', #19079 ) ;
#8091 = CARTESIAN_POINT ( 'NONE',  ( -19.41254052147348830, -26.35725562635142083, 28.76367750791695954 ) ) ;
#8092 = CARTESIAN_POINT ( 'NONE',  ( 1.035533905932739751, 61.50000000000000000, 47.15000000218494591 ) ) ;
#8093 = CARTESIAN_POINT ( 'NONE',  ( -14.83517299489735741, -28.99999999999998224, 19.36132249208304046 ) ) ;
#8094 = CARTESIAN_POINT ( 'NONE',  ( -15.00000000000000000, -32.50000000000000711, 1.500000000000000000 ) ) ;
#8095 = CARTESIAN_POINT ( 'NONE',  ( -19.24771351637089367, -21.35725562635142438, 19.13867750791695954 ) ) ;
#8096 = CARTESIAN_POINT ( 'NONE',  ( -7.999999999999986677, 68.00000000000000000, 45.00000000000000000 ) ) ;
#8097 = CARTESIAN_POINT ( 'NONE',  ( -10.75228648362910100, -26.64274437364854009, 32.26367750791695954 ) ) ;
#8098 = LINE ( 'NONE', #10923, #289 ) ;
#8099 = CARTESIAN_POINT ( 'NONE',  ( -10.58745947852648328, -26.35725562635138530, 18.48632249208304401 ) ) ;
#8100 = ADVANCED_FACE ( 'NONE', ( #5554 ), #17504, .F. ) ;
#8101 = CARTESIAN_POINT ( 'NONE',  ( 0.8561741729129460632, 66.06698729999999387, 45.50000000109247367 ) ) ;
#8102 = DIRECTION ( 'NONE',  ( 0.000000000000000000, 1.000000000000000000, 0.000000000000000000 ) ) ;
#8103 = DIRECTION ( 'NONE',  ( -2.775557561562890858E-16, 0.7071067811865454633, 0.7071067811865496822 ) ) ;
#8104 = EDGE_CURVE ( 'NONE', #10386, #3710, #14885, .T. ) ;
#8105 = CARTESIAN_POINT ( 'NONE',  ( 3.796994071234847710E-16, 61.93301269999999903, 46.75000000109246656 ) ) ;
#8106 = LINE ( 'NONE', #2306, #1445 ) ;
#8107 = CIRCLE ( 'NONE', #19047, 2.500000000000001776 ) ;
#8108 = VERTEX_POINT ( 'NONE', #11510 ) ;
#8109 = CARTESIAN_POINT ( 'NONE',  ( -12.95952864787948755, -30.95583473709188382, 34.89257249208303335 ) ) ;
#8110 = CARTESIAN_POINT ( 'NONE',  ( -17.64274437364858983, -19.75228648362910633, 5.798822492083041347 ) ) ;
#8111 = CARTESIAN_POINT ( 'NONE',  ( -17.51566270880201159, -22.35725562635141728, 34.88867750791696665 ) ) ;
#8112 = LINE ( 'NONE', #18700, #18022 ) ;
#8113 = CARTESIAN_POINT ( 'NONE',  ( -20.00369391078757886, -29.24501739517668142, 20.01757249208303691 ) ) ;
#8114 = AXIS2_PLACEMENT_3D ( 'NONE', #698, #9415, #18642 ) ;
#8115 = CARTESIAN_POINT ( 'NONE',  ( -1.265664690411616068E-16, 66.06698730000000808, 47.75000000109246656 ) ) ;
#8116 = ORIENTED_EDGE ( 'NONE', *, *, #7816, .T. ) ;
#8117 = EDGE_CURVE ( 'NONE', #7050, #8090, #1042, .T. ) ;
#8118 = ORIENTED_EDGE ( 'NONE', *, *, #18199, .F. ) ;
#8119 = VECTOR ( 'NONE', #13873, 1000.000000000000000 ) ;
#8120 = DIRECTION ( 'NONE',  ( 0.000000000000000000, 0.000000000000000000, 1.000000000000000000 ) ) ;
#8121 = DIRECTION ( 'NONE',  ( 1.000000000000000000, -0.000000000000000000, -0.000000000000000000 ) ) ;
#8122 = LINE ( 'NONE', #1847, #16892 ) ;
#8123 = LINE ( 'NONE', #18329, #3112 ) ;
#8124 = LINE ( 'NONE', #14096, #16002 ) ;
#8125 = EDGE_CURVE ( 'NONE', #535, #5700, #6128, .T. ) ;
#8126 = CARTESIAN_POINT ( 'NONE',  ( 1.844224359752661968, -38.39960408384397539, 3.000000000000000000 ) ) ;
#8127 = AXIS2_PLACEMENT_3D ( 'NONE', #5092, #7935, #9293 ) ;
#8128 = CARTESIAN_POINT ( 'NONE',  ( 50.00000000000000000, 3.000000000000000000, -60.00000000000000000 ) ) ;
#8129 = ORIENTED_EDGE ( 'NONE', *, *, #17399, .F. ) ;
#8130 = ORIENTED_EDGE ( 'NONE', *, *, #656, .F. ) ;
#8131 = CARTESIAN_POINT ( 'NONE',  ( -15.16482700510258574, -30.99999999999998224, 33.13867750791695954 ) ) ;
#8132 = ORIENTED_EDGE ( 'NONE', *, *, #19335, .T. ) ;
#8133 = AXIS2_PLACEMENT_3D ( 'NONE', #14397, #5483, #13212 ) ;
#8135 = ORIENTED_EDGE ( 'NONE', *, *, #15515, .T. ) ;
#8134 = ORIENTED_EDGE ( 'NONE', *, *, #12757, .T. ) ;
#8136 = CARTESIAN_POINT ( 'NONE',  ( -12.48433729119799196, -22.35725562635139596, 38.61132249208304046 ) ) ;
#8137 = CARTESIAN_POINT ( 'NONE',  ( -17.04047135212043784, -30.95583473709190159, 12.35742750791695777 ) ) ;
#8138 =( BOUNDED_CURVE ( )  B_SPLINE_CURVE ( 2, ( #5909, #14831, #17874, #4447, #17969, #16397, #8940, #6015, #1604 ),
 .UNSPECIFIED., .F., .T. ) 
 B_SPLINE_CURVE_WITH_KNOTS ( ( 3, 2, 2, 2, 3 ),
 ( 0.2142857142857140795, 0.2321428571428570675, 0.2500000000000000000, 0.2678571428571429602, 0.2857142857142859205 ),
 .UNSPECIFIED. ) 
 CURVE ( )  GEOMETRIC_REPRESENTATION_ITEM ( )  RATIONAL_B_SPLINE_CURVE ( ( 1.000000000000000888, 0.9238795325112859613, 1.000000000000000000, 0.9238795325112867385, 1.000000000000000000, 0.9238795325112867385, 1.000000000000000000, 0.9238795325112857393, 1.000000000000000888 ) ) 
 REPRESENTATION_ITEM ( '' )  );
#8139 = CARTESIAN_POINT ( 'NONE',  ( -1.035533905932738641, 66.50000000000000000, 47.44999999999998863 ) ) ;
#8140 = CARTESIAN_POINT ( 'NONE',  ( -1.035533905932738641, 66.50000000000000000, 47.55000000218494449 ) ) ;
#8141 = CARTESIAN_POINT ( 'NONE',  ( -15.00000000000000000, 35.00000000000000000, 0.000000000000000000 ) ) ;
#8142 = ORIENTED_EDGE ( 'NONE', *, *, #15071, .T. ) ;
#8143 = CARTESIAN_POINT ( 'NONE',  ( -15.16482700510260706, -26.99999999999998579, 27.88867750791696309 ) ) ;
#8144 = AXIS2_PLACEMENT_3D ( 'NONE', #8825, #3040, #14810 ) ;
#8145 = SURFACE_SIDE_STYLE ('',( #12349 ) ) ;
#8146 = VERTEX_POINT ( 'NONE', #10047 ) ;
#8147 = CARTESIAN_POINT ( 'NONE',  ( -0.1250000000000104083, 33.84386001800125143, 52.64142135623733765 ) ) ;
#8148 = ORIENTED_EDGE ( 'NONE', *, *, #5536, .T. ) ;
#8149 = DIRECTION ( 'NONE',  ( 0.000000000000000000, 0.000000000000000000, -1.000000000000000000 ) ) ;
#8150 = FACE_OUTER_BOUND ( 'NONE', #9426, .T. ) ;
#8151 = LINE ( 'NONE', #4926, #16585 ) ;
#8152 = CIRCLE ( 'NONE', #3459, 6.799999999999999822 ) ;
#8153 = CARTESIAN_POINT ( 'NONE',  ( -25.00000000000000000, 53.00000000000000711, 30.00000000000000000 ) ) ;
#8154 = CARTESIAN_POINT ( 'NONE',  ( -2.066987300000001415, 64.85617417291294373, 48.10000000109246798 ) ) ;
#8155 = CARTESIAN_POINT ( 'NONE',  ( -40.00000000000000711, 113.0000000000000000, -24.49999999999999289 ) ) ;
#8156 = DIRECTION ( 'NONE',  ( -0.9863224920830415687, -5.704848896154130918E-15, -0.1648270051026189120 ) ) ;
#8157 = VECTOR ( 'NONE', #13858, 1000.000000000000000 ) ;
#8158 = DIRECTION ( 'NONE',  ( -0.000000000000000000, 0.000000000000000000, 1.000000000000000000 ) ) ;
#8159 = ORIENTED_EDGE ( 'NONE', *, *, #6526, .F. ) ;
#8160 = CARTESIAN_POINT ( 'NONE',  ( -13.82508104294698192, -29.04416526290806644, 27.66992750791695244 ) ) ;
#8161 = LINE ( 'NONE', #2083, #12711 ) ;
#8162 = ORIENTED_EDGE ( 'NONE', *, *, #15550, .F. ) ;
#8163 = VECTOR ( 'NONE', #2134, 1000.000000000000000 ) ;
#8164 = CARTESIAN_POINT ( 'NONE',  ( -19.41254052147350961, -21.64274437364857562, 26.36132249208304401 ) ) ;
#8165 = AXIS2_PLACEMENT_3D ( 'NONE', #4707, #9003, #16366 ) ;
#8166 = CARTESIAN_POINT ( 'NONE',  ( 1.767766952966369987, 65.76776695296638309, 45.69999999999999574 ) ) ;
#8167 = CARTESIAN_POINT ( 'NONE',  ( -11.99999999999999289, -23.83517299489735564, 33.79882249208304756 ) ) ;
#8168 = CARTESIAN_POINT ( 'NONE',  ( -41.00000000000000711, 53.00000000000000711, -38.50000000000000711 ) ) ;
#8169 = ORIENTED_EDGE ( 'NONE', *, *, #9778, .F. ) ;
#8170 = AXIS2_PLACEMENT_3D ( 'NONE', #4942, #10899, #12284 ) ;
#8171 = LINE ( 'NONE', #6508, #5615 ) ;
#8172 = ORIENTED_EDGE ( 'NONE', *, *, #757, .F. ) ;
#8173 = CARTESIAN_POINT ( 'NONE',  ( -47.00000000000002132, 115.0000000000000000, -57.00000000000001421 ) ) ;
#8174 = EDGE_CURVE ( 'NONE', #1049, #9, #7563, .T. ) ;
#8175 = ADVANCED_FACE ( 'NONE', ( #14280 ), #8586, .F. ) ;
#8176 = CARTESIAN_POINT ( 'NONE',  ( -41.00000000000000711, 53.00000000000000711, 27.50000000000000000 ) ) ;
#8177 = DIRECTION ( 'NONE',  ( 1.000000000000000000, 0.000000000000000000, 0.000000000000000000 ) ) ;
#8178 = AXIS2_PLACEMENT_3D ( 'NONE', #236, #6220, #8856 ) ;
#8179 = EDGE_CURVE ( 'NONE', #14706, #18337, #11483, .T. ) ;
#8180 = CIRCLE ( 'NONE', #38, 5.800000000000007816 ) ;
#8181 = FILL_AREA_STYLE ('',( #18186 ) ) ;
#8182 = DIRECTION ( 'NONE',  ( 0.000000000000000000, 9.912705577010328508E-16, 1.000000000000000000 ) ) ;
#8184 = ADVANCED_FACE ( 'NONE', ( #14768 ), #7613, .F. ) ;
#8183 = DIRECTION ( 'NONE',  ( 0.000000000000000000, 1.000000000000000000, 0.000000000000000000 ) ) ;
#8185 = DIRECTION ( 'NONE',  ( 0.7071067811865561215, 0.4999999999999953926, -0.4999999999999925060 ) ) ;
#8186 = VECTOR ( 'NONE', #1971, 1000.000000000000000 ) ;
#8187 = ORIENTED_EDGE ( 'NONE', *, *, #1225, .F. ) ;
#8188 = CIRCLE ( 'NONE', #17262, 1.280000000000000027 ) ;
#8189 = CARTESIAN_POINT ( 'NONE',  ( -11.21908421996108629, -20.46040770435011069, 25.91992750791694888 ) ) ;
#8190 = CARTESIAN_POINT ( 'NONE',  ( -1.035533905932738641, 66.50000000000000000, 44.35000000218493454 ) ) ;
#8191 = ADVANCED_FACE ( 'NONE', ( #14862 ), #10339, .T. ) ;
#8192 = CARTESIAN_POINT ( 'NONE',  ( -17.64274437364858983, -19.75228648362910633, 37.29882249208303335 ) ) ;
#8193 = VECTOR ( 'NONE', #5208, 1000.000000000000000 ) ;
#8194 = LINE ( 'NONE', #3482, #10706 ) ;
#8195 = CARTESIAN_POINT ( 'NONE',  ( -10.04416526290807710, -25.50457296725819489, 37.29492750791697375 ) ) ;
#8196 = VECTOR ( 'NONE', #13480, 1000.000000000000000 ) ;
#8197 = CARTESIAN_POINT ( 'NONE',  ( 0.000000000000000000, 64.00000000000000000, 49.99999999999999289 ) ) ;
#8198 = CARTESIAN_POINT ( 'NONE',  ( -9.999999999999994671, -24.16482700510257686, 31.82617750791696309 ) ) ;
#8199 = CARTESIAN_POINT ( 'NONE',  ( -1.040834085586084257E-14, 29.74264068711925901, 56.74264068711929809 ) ) ;
#8200 = CARTESIAN_POINT ( 'NONE',  ( -11.21908421996106142, -27.53959229564982181, 23.95507249208304046 ) ) ;
#8201 = EDGE_CURVE ( 'NONE', #6401, #3007, #10537, .T. ) ;
#8202 = CARTESIAN_POINT ( 'NONE',  ( -1.035533905932738863, 61.50000000000000000, 48.54999999999999716 ) ) ;
#8203 = CARTESIAN_POINT ( 'NONE',  ( -0.1250000000000104083, 33.84290755733280776, 52.64142146683631296 ) ) ;
#8204 = DIRECTION ( 'NONE',  ( 1.000000000000000000, 0.000000000000000000, 0.000000000000000000 ) ) ;
#8205 = VECTOR ( 'NONE', #4676, 1000.000000000000000 ) ;
#8206 = CARTESIAN_POINT ( 'NONE',  ( -2.066987300000001859, 64.85617417291294373, 44.90000000109247225 ) ) ;
#8207 = LINE ( 'NONE', #5073, #10165 ) ;
#8208 = VECTOR ( 'NONE', #15680, 1000.000000000000000 ) ;
#8209 = EDGE_LOOP ( 'NONE', ( #2273, #16141, #18921, #9006 ) ) ;
#8210 = EDGE_CURVE ( 'NONE', #5477, #7059, #8679, .T. ) ;
#8211 = DIRECTION ( 'NONE',  ( 0.000000000000000000, -1.000000000000000000, 0.000000000000000000 ) ) ;
#8212 = EDGE_CURVE ( 'NONE', #12337, #14902, #13577, .T. ) ;
#8213 = CARTESIAN_POINT ( 'NONE',  ( -15.96867458239597326, -26.95583473709190159, 22.85742750791695954 ) ) ;
#8214 = DIRECTION ( 'NONE',  ( 0.000000000000000000, 0.000000000000000000, -1.000000000000000000 ) ) ;
#8215 = ADVANCED_FACE ( 'NONE', ( #11709, #68 ), #159, .T. ) ;
#8216 = CARTESIAN_POINT ( 'NONE',  ( -18.64274437364860049, -18.02023567606023491, 32.04882249208304046 ) ) ;
#8217 = CARTESIAN_POINT ( 'NONE',  ( 2.066987300000001415, 64.00000000000000000, 47.55000000109247082 ) ) ;
#8218 = EDGE_LOOP ( 'NONE', ( #1045, #3244, #871, #13019 ) ) ;
#8219 = ORIENTED_EDGE ( 'NONE', *, *, #14433, .F. ) ;
#8220 = ADVANCED_FACE ( 'NONE', ( #7213 ), #9075, .F. ) ;
#8221 = AXIS2_PLACEMENT_3D ( 'NONE', #8576, #11408, #1126 ) ;
#8222 = DIRECTION ( 'NONE',  ( -1.000000000000000000, -0.000000000000000000, -0.000000000000000000 ) ) ;
#8223 = CARTESIAN_POINT ( 'NONE',  ( -40.00000000000000711, 113.0000000000000000, -12.49999999999999645 ) ) ;
#8224 = CARTESIAN_POINT ( 'NONE',  ( 1.461580736456473684, 65.46158073645646880, 45.25000000109247367 ) ) ;
#8225 = DIRECTION ( 'NONE',  ( 0.000000000000000000, 0.000000000000000000, 1.000000000000000000 ) ) ;
#8226 = CARTESIAN_POINT ( 'NONE',  ( -2.500000000000001776, 64.00000000000000000, 49.99999999999999289 ) ) ;
#8227 = LINE ( 'NONE', #18331, #6305 ) ;
#8228 = DIRECTION ( 'NONE',  ( -0.000000000000000000, -0.000000000000000000, -1.000000000000000000 ) ) ;
#8229 = EDGE_CURVE ( 'NONE', #2670, #4095, #11933, .T. ) ;
#8230 = ORIENTED_EDGE ( 'NONE', *, *, #7592, .T. ) ;
#8231 = ORIENTED_EDGE ( 'NONE', *, *, #6066, .F. ) ;
#8232 = CARTESIAN_POINT ( 'NONE',  ( -9.754982604823348780, -18.99630608921234654, 36.41992750791695954 ) ) ;
#8233 = ORIENTED_EDGE ( 'NONE', *, *, #3894, .T. ) ;
#8235 = ORIENTED_EDGE ( 'NONE', *, *, #13597, .F. ) ;
#8234 = ORIENTED_EDGE ( 'NONE', *, *, #8212, .F. ) ;
#8236 = CARTESIAN_POINT ( 'NONE',  ( -16.64274437364858272, -21.48433729119797420, 26.79882249208304401 ) ) ;
#8237 = CARTESIAN_POINT ( 'NONE',  ( -18.64274437364853654, -29.97976432393976509, 17.82617750791695954 ) ) ;
#8238 = DIRECTION ( 'NONE',  ( -0.000000000000000000, -1.000000000000000000, -0.000000000000000000 ) ) ;
#8239 = CARTESIAN_POINT ( 'NONE',  ( 1.035533905932738197, 66.50000000000000000, 49.05000000218495160 ) ) ;
#8240 = CARTESIAN_POINT ( 'NONE',  ( 1.753982408753060440, -45.28611686177728046, 3.000000000000000000 ) ) ;
#8241 = ORIENTED_EDGE ( 'NONE', *, *, #8785, .F. ) ;
#8242 = CARTESIAN_POINT ( 'NONE',  ( -12.68318583509884157, -21.92450931948787485, 31.16992750791695954 ) ) ;
#8243 = CARTESIAN_POINT ( 'NONE',  ( -1.485306817036799787, 0.000000000000000000, 7.499999999999995559 ) ) ;
#8244 = ORIENTED_EDGE ( 'NONE', *, *, #9739, .T. ) ;
#8245 = CARTESIAN_POINT ( 'NONE',  ( -40.00000000000000000, 53.00000000000000711, 30.00000000000000000 ) ) ;
#8246 = ORIENTED_EDGE ( 'NONE', *, *, #15244, .F. ) ;
#8247 = DIRECTION ( 'NONE',  ( 1.000000000000000000, 0.000000000000000000, 0.000000000000000000 ) ) ;
#8248 = CARTESIAN_POINT ( 'NONE',  ( -2.500000000000001776, 64.00000000000000000, 45.19999999999999574 ) ) ;
#8249 = DIRECTION ( 'NONE',  ( 0.000000000000000000, 1.632680918566406793E-16, -1.000000000000000000 ) ) ;
#8250 = CARTESIAN_POINT ( 'NONE',  ( -2.066987300000000971, 63.14382582708704916, 49.00000000109246656 ) ) ;
#8251 = DIRECTION ( 'NONE',  ( -1.000000000000000000, 0.000000000000000000, -0.000000000000000000 ) ) ;
#8252 = CARTESIAN_POINT ( 'NONE',  ( 2.500000000000000000, -1.178949249685214307, 2.042000000000002036 ) ) ;
#8253 = DIRECTION ( 'NONE',  ( -1.000000000000000000, -0.000000000000000000, -0.000000000000000000 ) ) ;
#8254 = EDGE_CURVE ( 'NONE', #15143, #13986, #10436, .T. ) ;
#8255 = ORIENTED_EDGE ( 'NONE', *, *, #4029, .F. ) ;
#8256 = VERTEX_POINT ( 'NONE', #13380 ) ;
#8257 = CARTESIAN_POINT ( 'NONE',  ( -20.04416526290808065, -25.17491895705300209, 28.98242750791695244 ) ) ;
#8258 =( BOUNDED_SURFACE ( )  B_SPLINE_SURFACE ( 1, 2, ( 
 ( #18814, #2251, #3905, #3624, #863, #8239, #6942, #12911, #3715, #11063, #9873, #6756, #15584, #15867, #8324, #14206, #772, #12724, #14113, #9594, #5387, #6842, #12815, #13002, #14295, #2427, #18813, #18720, #5198, #8411, #18631, #2152, #15961, #11344, #14386, #8140, #18907, #11436, #5284, #17430, #687, #4000, #9959, #17336, #11155, #6671, #962, #2525, #14484, #17153, #5473, #12634, #8508, #1055, #11243, #19003, #7034, #17062, #17246, #9688, #15681, #3816, #9782, #15775, #2341, #2818, #17822, #8601, #4298, #13394, #1355, #7527, #5668, #11527, #10454, #11725, #17927, #1255, #2721, #10152, #5865, #11632, #16152, #8892, #4499, #7131, #11935, #13099, #14978, #17721, #5964, #10255, #1454, #7427, #16448, #19390, #7327, #13294, #3015, #14583, #19098 ),
 ( #8991, #19296, #14787, #8694, #5762, #1552, #13502, #14678, #11825, #7232, #4399, #1154, #5569, #10360, #13202, #16354, #17621, #4198, #17521, #16245, #2918, #19195, #8799, #14882, #10061, #4101, #16055, #2615, #1656, #18024, #13794, #9378, #16845, #467, #7827, #13594, #6165, #10851, #12026, #4694, #270, #4597, #9479, #12422, #374, #15083, #6063, #15179, #3407, #16947, #6455, #2033, #9094, #9191, #1747, #83, #3114, #8026, #10945, #10555, #10651, #7630, #18224, #6361, #180, #1841, #3511, #15272, #15372, #15465, #7731, #12125, #1946, #18120, #16654, #16544, #13693, #18420, #12324, #3219, #6258, #12223, #13891, #4800, #10749, #16746, #3318, #9286, #18320, #4890, #7928, #4986, #3597, #2576, #16199, #15913, #14441, #2476, #12517, #8464, #1104 ) ),
 .UNSPECIFIED., .F., .F., .F. ) 
 B_SPLINE_SURFACE_WITH_KNOTS ( ( 2, 2 ),
 ( 3, 2, 2, 2, 2, 2, 2, 2, 2, 2, 2, 2, 2, 2, 2, 2, 2, 2, 2, 2, 2, 2, 2, 2, 2, 2, 2, 2, 2, 2, 2, 2, 2, 2, 2, 2, 2, 2, 2, 2, 2, 2, 2, 2, 2, 2, 2, 2, 2, 2, 3 ),
 ( 0.000000000000000000, 1.000000000000000000 ),
 ( 0.000000000000000000, 0.01785714285714285615, 0.03571428571428571230, 0.05357142857142856845, 0.07142857142857142461, 0.08928571428571428770, 0.1071428571428571369, 0.1250000000000000000, 0.1428571428571428492, 0.1607142857142857262, 0.1785714285714285754, 0.1964285714285714246, 0.2142857142857142738, 0.2321428571428571508, 0.2500000000000000000, 0.2678571428571428492, 0.2857142857142856984, 0.3035714285714285476, 0.3214285714285714524, 0.3392857142857143016, 0.3571428571428571508, 0.3750000000000000000, 0.3928571428571428492, 0.4107142857142856984, 0.4285714285714285476, 0.4464285714285714524, 0.4642857142857143016, 0.4821428571428571508, 0.5000000000000000000, 0.5178571428571429047, 0.5357142857142856984, 0.5535714285714286031, 0.5714285714285713969, 0.5892857142857143016, 0.6071428571428570953, 0.6250000000000000000, 0.6428571428571429047, 0.6607142857142856984, 0.6785714285714286031, 0.6964285714285713969, 0.7142857142857143016, 0.7321428571428570953, 0.7500000000000000000, 0.7678571428571429047, 0.7857142857142856984, 0.8035714285714286031, 0.8214285714285713969, 0.8392857142857143016, 0.8571428571428570953, 0.8750000000000000000, 0.8928571428571429047 ),
 .UNSPECIFIED. ) 
 GEOMETRIC_REPRESENTATION_ITEM ( )  RATIONAL_B_SPLINE_SURFACE ( (
 ( 1.000000000000000000, 0.9238795325112867385, 1.000000000000000000, 0.9238795325112867385, 1.000000000000000000, 0.9238795325112867385, 1.000000000000000000, 0.9238795325112867385, 1.000000000000000000, 0.9238795325112867385, 1.000000000000000000, 0.9238795325112867385, 1.000000000000000000, 0.9238795325112867385, 1.000000000000000000, 0.9238795325112867385, 1.000000000000000000, 0.9238795325112867385, 1.000000000000000000, 0.9238795325112867385, 1.000000000000000000, 0.9238795325112867385, 1.000000000000000000, 0.9238795325112867385, 1.000000000000000000, 0.9238795325112867385, 1.000000000000000000, 0.9238795325112867385, 1.000000000000000000, 0.9238795325112867385, 1.000000000000000000, 0.9238795325112867385, 1.000000000000000000, 0.9238795325112867385, 1.000000000000000000, 0.9238795325112867385, 1.000000000000000000, 0.9238795325112867385, 1.000000000000000000, 0.9238795325112867385, 1.000000000000000000, 0.9238795325112867385, 1.000000000000000000, 0.9238795325112867385, 1.000000000000000000, 0.9238795325112867385, 1.000000000000000000, 0.9238795325112867385, 1.000000000000000000, 0.9238795325112867385, 1.000000000000000000, 0.9238795325112867385, 1.000000000000000000, 0.9238795325112867385, 1.000000000000000000, 0.9238795325112867385, 1.000000000000000000, 0.9238795325112867385, 1.000000000000000000, 0.9238795325112867385, 1.000000000000000000, 0.9238795325112867385, 1.000000000000000000, 0.9238795325112867385, 1.000000000000000000, 0.9238795325112867385, 1.000000000000000000, 0.9238795325112867385, 1.000000000000000000, 0.9238795325112867385, 1.000000000000000000, 0.9238795325112867385, 1.000000000000000000, 0.9238795325112867385, 1.000000000000000000, 0.9238795325112867385, 1.000000000000000000, 0.9238795325112867385, 1.000000000000000000, 0.9238795325112867385, 1.000000000000000000, 0.9238795325112867385, 1.000000000000000000, 0.9238795325112867385, 1.000000000000000000, 0.9238795325112867385, 1.000000000000000000, 0.9238795325112867385, 1.000000000000000000, 0.9238795325112867385, 1.000000000000000000, 0.9238795325112867385, 1.000000000000000000, 0.9238795325112867385, 1.000000000000000000, 0.9238795325112867385, 1.000000000000000000, 0.9238795325112867385, 1.000000000000000000, 0.9238795325112867385, 1.000000000000000000),
 ( 1.000000000000000000, 0.9238795325112867385, 1.000000000000000000, 0.9238795325112867385, 1.000000000000000000, 0.9238795325112867385, 1.000000000000000000, 0.9238795325112867385, 1.000000000000000000, 0.9238795325112867385, 1.000000000000000000, 0.9238795325112867385, 1.000000000000000000, 0.9238795325112867385, 1.000000000000000000, 0.9238795325112867385, 1.000000000000000000, 0.9238795325112867385, 1.000000000000000000, 0.9238795325112867385, 1.000000000000000000, 0.9238795325112867385, 1.000000000000000000, 0.9238795325112867385, 1.000000000000000000, 0.9238795325112867385, 1.000000000000000000, 0.9238795325112867385, 1.000000000000000000, 0.9238795325112867385, 1.000000000000000000, 0.9238795325112867385, 1.000000000000000000, 0.9238795325112867385, 1.000000000000000000, 0.9238795325112867385, 1.000000000000000000, 0.9238795325112867385, 1.000000000000000000, 0.9238795325112867385, 1.000000000000000000, 0.9238795325112867385, 1.000000000000000000, 0.9238795325112867385, 1.000000000000000000, 0.9238795325112867385, 1.000000000000000000, 0.9238795325112867385, 1.000000000000000000, 0.9238795325112867385, 1.000000000000000000, 0.9238795325112867385, 1.000000000000000000, 0.9238795325112867385, 1.000000000000000000, 0.9238795325112867385, 1.000000000000000000, 0.9238795325112867385, 1.000000000000000000, 0.9238795325112867385, 1.000000000000000000, 0.9238795325112867385, 1.000000000000000000, 0.9238795325112867385, 1.000000000000000000, 0.9238795325112867385, 1.000000000000000000, 0.9238795325112867385, 1.000000000000000000, 0.9238795325112867385, 1.000000000000000000, 0.9238795325112867385, 1.000000000000000000, 0.9238795325112867385, 1.000000000000000000, 0.9238795325112867385, 1.000000000000000000, 0.9238795325112867385, 1.000000000000000000, 0.9238795325112867385, 1.000000000000000000, 0.9238795325112867385, 1.000000000000000000, 0.9238795325112867385, 1.000000000000000000, 0.9238795325112867385, 1.000000000000000000, 0.9238795325112867385, 1.000000000000000000, 0.9238795325112867385, 1.000000000000000000, 0.9238795325112867385, 1.000000000000000000, 0.9238795325112867385, 1.000000000000000000, 0.9238795325112867385, 1.000000000000000000, 0.9238795325112867385, 1.000000000000000000, 0.9238795325112867385, 1.000000000000000000) ) ) 
 REPRESENTATION_ITEM ( '' )  SURFACE ( )  );
#8259 = DIRECTION ( 'NONE',  ( -1.000000000000000000, 0.000000000000000000, -0.000000000000000000 ) ) ;
#8260 = EDGE_LOOP ( 'NONE', ( #7161, #17171, #11662, #12090 ) ) ;
#8261 = CARTESIAN_POINT ( 'NONE',  ( -14.83517299489735741, -28.99999999999998224, 35.11132249208304046 ) ) ;
#8262 = DIRECTION ( 'NONE',  ( 0.000000000000000000, -1.000000000000000000, 0.000000000000000000 ) ) ;
#8263 = CARTESIAN_POINT ( 'NONE',  ( -17.51566270880199738, -25.64274437364856496, 30.73632249208304401 ) ) ;
#8264 = ORIENTED_EDGE ( 'NONE', *, *, #5536, .F. ) ;
#8265 = DIRECTION ( 'NONE',  ( 1.000000000000000000, 0.000000000000000000, 0.000000000000000000 ) ) ;
#8266 = VERTEX_POINT ( 'NONE', #10136 ) ;
#8267 = CARTESIAN_POINT ( 'NONE',  ( 1.767766984964166399, 65.76776692096858312, 45.00000000000000000 ) ) ;
#8268 = CARTESIAN_POINT ( 'NONE',  ( -25.00000000000000000, 53.00000000000000711, 30.00000000000000000 ) ) ;
#8269 = CARTESIAN_POINT ( 'NONE',  ( 2.500000000000001776, 64.00000000000000000, 45.70000000218494307 ) ) ;
#8270 = FACE_BOUND ( 'NONE', #1274, .T. ) ;
#8271 = FILL_AREA_STYLE ('',( #6980 ) ) ;
#8272 = CARTESIAN_POINT ( 'NONE',  ( 8.000000000000014211, 60.00000000000000711, 66.99999999999997158 ) ) ;
#8273 = FACE_OUTER_BOUND ( 'NONE', #16070, .T. ) ;
#8274 = UNCERTAINTY_MEASURE_WITH_UNIT (LENGTH_MEASURE( 1.000000000000000082E-05 ), #12904, 'distance_accuracy_value', 'NONE');
#8275 = ORIENTED_EDGE ( 'NONE', *, *, #8117, .F. ) ;
#8276 = CARTESIAN_POINT ( 'NONE',  ( -10.75228648362910100, -26.64274437364854009, 32.26367750791695954 ) ) ;
#8277 = CARTESIAN_POINT ( 'NONE',  ( 2.066987300000001859, 64.85617417291294373, 46.80000000109246372 ) ) ;
#8278 = CARTESIAN_POINT ( 'NONE',  ( -13.82508104294702100, -18.95583473709188382, 37.95507249208304756 ) ) ;
#8279 = VECTOR ( 'NONE', #7591, 1000.000000000000000 ) ;
#8280 = LINE ( 'NONE', #2578, #3444 ) ;
#8281 = CARTESIAN_POINT ( 'NONE',  ( -19.95583473709191580, -22.49542703274176603, 24.16992750791694888 ) ) ;
#8282 = DIRECTION ( 'NONE',  ( 0.000000000000000000, 0.000000000000000000, -1.000000000000000000 ) ) ;
#8283 = CARTESIAN_POINT ( 'NONE',  ( -16.50457296725820555, -28.95583473709189803, 33.35742750791695954 ) ) ;
#8284 = CARTESIAN_POINT ( 'NONE',  ( -24.00000000000000000, 47.00000000000000711, -50.00000000000000000 ) ) ;
#8285 = CARTESIAN_POINT ( 'NONE',  ( -19.95583473709190514, -25.50457296725823042, 30.95507249208304046 ) ) ;
#8286 = CARTESIAN_POINT ( 'NONE',  ( -1.461580736456473462, 62.53841926354353120, 45.05000000109246372 ) ) ;
#8287 = CARTESIAN_POINT ( 'NONE',  ( -5.799326430397249155, 29.83055285973289372, 56.65377616443620212 ) ) ;
#8288 = CYLINDRICAL_SURFACE ( 'NONE', #6176, 1.599999999999997202 ) ;
#8289 = CARTESIAN_POINT ( 'NONE',  ( -1.035533905932738863, 61.50000000000000000, 48.54999999999999716 ) ) ;
#8290 = LINE ( 'NONE', #6722, #17406 ) ;
#8291 = AXIS2_PLACEMENT_3D ( 'NONE', #18096, #16523, #10530 ) ;
#8292 = VERTEX_POINT ( 'NONE', #7508 ) ;
#8293 = EDGE_CURVE ( 'NONE', #13385, #11368, #19374, .T. ) ;
#8294 =( NAMED_UNIT ( * ) SI_UNIT ( $, .STERADIAN. ) SOLID_ANGLE_UNIT ( ) );
#8295 = CARTESIAN_POINT ( 'NONE',  ( -1.461580736456473906, 65.46158073645646880, 45.45000000109246940 ) ) ;
#8296 = CARTESIAN_POINT ( 'NONE',  ( -17.95583473709191580, -23.03132541760400898, 39.91992750791695954 ) ) ;
#8297 = PLANE ( 'NONE',  #999 ) ;
#8298 = CARTESIAN_POINT ( 'NONE',  ( -11.35725562635139418, -29.97976432393972601, 39.92382249208304046 ) ) ;
#8299 = CARTESIAN_POINT ( 'NONE',  ( 0.8561741729129460632, 66.06698729999999387, 45.30000000109247082 ) ) ;
#8300 = EDGE_LOOP ( 'NONE', ( #3818, #12808, #11927, #9311, #11454, #17237 ) ) ;
#8301 = CARTESIAN_POINT ( 'NONE',  ( -15.20357423236093375, -43.78611686177728046, 1.500000000000000000 ) ) ;
#8302 = DIRECTION ( 'NONE',  ( -1.156482317317871478E-16, 1.000000000000000000, 0.000000000000000000 ) ) ;
#8303 = VECTOR ( 'NONE', #17281, 1000.000000000000000 ) ;
#8304 = CARTESIAN_POINT ( 'NONE',  ( -41.00000000000000711, 110.0000000000000000, -11.50000000000000000 ) ) ;
#8305 = DIRECTION ( 'NONE',  ( -3.491481338843133355E-15, -0.7071067811865495711, 0.7071067811865454633 ) ) ;
#8306 = CARTESIAN_POINT ( 'NONE',  ( -32.50000000000000000, 52.00000000000000711, 15.00000000000000000 ) ) ;
#8307 = ADVANCED_FACE ( 'NONE', ( #5945 ), #11916, .F. ) ;
#8308 = EDGE_CURVE ( 'NONE', #535, #17001, #17703, .T. ) ;
#8309 = CARTESIAN_POINT ( 'NONE',  ( 32.50000000000000000, 52.00000000000000711, 15.00000000000000000 ) ) ;
#8310 = ADVANCED_FACE ( 'NONE', ( #4482 ), #4282, .F. ) ;
#8311 = DIRECTION ( 'NONE',  ( 2.220446049250313081E-16, 0.7071067811865452413, 0.7071067811865497932 ) ) ;
#8312 = EDGE_LOOP ( 'NONE', ( #5259, #17352, #2147, #2333 ) ) ;
#8313 = ORIENTED_EDGE ( 'NONE', *, *, #958, .T. ) ;
#8314 = CARTESIAN_POINT ( 'NONE',  ( -7.999999999999996447, -23.83517299489733432, 2.298822492083038682 ) ) ;
#8315 = AXIS2_PLACEMENT_3D ( 'NONE', #17170, #15882, #14403 ) ;
#8316 = SHAPE_REPRESENTATION_RELATIONSHIP ( 'NONE' , 'NONE' ,  #12005, #1517 ) ;
#8317 = EDGE_LOOP ( 'NONE', ( #14490, #10969, #4318, #5380 ) ) ;
#8318 = VECTOR ( 'NONE', #3691, 1000.000000000000000 ) ;
#8320 = ORIENTED_EDGE ( 'NONE', *, *, #4037, .F. ) ;
#8319 = ORIENTED_EDGE ( 'NONE', *, *, #17872, .T. ) ;
#8321 = CARTESIAN_POINT ( 'NONE',  ( -16.35725562635141372, -26.68048971390461332, 35.54882249208304046 ) ) ;
#8322 = CARTESIAN_POINT ( 'NONE',  ( -8.044165262908075320, -26.04047135212042718, 26.79492750791695954 ) ) ;
#8323 = DIRECTION ( 'NONE',  ( 1.000000000000000000, 0.000000000000000000, 0.000000000000000000 ) ) ;
#8324 = CARTESIAN_POINT ( 'NONE',  ( -1.767766952966369765, 62.23223304703363112, 48.60000000218494165 ) ) ;
#8325 = CARTESIAN_POINT ( 'NONE',  ( -7.999999999999986677, 60.00000000000000711, 45.00000000000000000 ) ) ;
#8326 = EDGE_LOOP ( 'NONE', ( #2967, #18535, #1833, #15792 ) ) ;
#8327 = CARTESIAN_POINT ( 'NONE',  ( 2.500000000000000000, 1.178949249685212974, -2.042000000000001148 ) ) ;
#8328 = ORIENTED_EDGE ( 'NONE', *, *, #4349, .T. ) ;
#8329 = CARTESIAN_POINT ( 'NONE',  ( 44.99999999999998579, 0.000000000000000000, -56.59999999999998010 ) ) ;
#8330 = ORIENTED_EDGE ( 'NONE', *, *, #14647, .T. ) ;
#8331 = DIRECTION ( 'NONE',  ( -1.000000000000000000, 0.000000000000000000, 0.000000000000000000 ) ) ;
#8332 = FACE_OUTER_BOUND ( 'NONE', #363, .T. ) ;
#8333 = AXIS2_PLACEMENT_3D ( 'NONE', #2415, #12529, #8399 ) ;
#8334 = CARTESIAN_POINT ( 'NONE',  ( -2.066987300000001859, 64.85617417291294373, 46.30000000109247082 ) ) ;
#8335 = EDGE_CURVE ( 'NONE', #16872, #18667, #1338, .T. ) ;
#8336 = VECTOR ( 'NONE', #648, 1000.000000000000000 ) ;
#8337 = CARTESIAN_POINT ( 'NONE',  ( -2.066987300000001415, 64.00000000000000000, 49.75000000109246656 ) ) ;
#8338 = FACE_OUTER_BOUND ( 'NONE', #6182, .T. ) ;
#8339 = PLANE ( 'NONE',  #13308 ) ;
#8340 = CARTESIAN_POINT ( 'NONE',  ( 11.00000000000003020, 60.00000000000000711, 63.99999999999994316 ) ) ;
#8341 = EDGE_LOOP ( 'NONE', ( #14213, #1407, #8148, #17870 ) ) ;
#8342 = ORIENTED_EDGE ( 'NONE', *, *, #8533, .F. ) ;
#8343 = CARTESIAN_POINT ( 'NONE',  ( -11.21908421996108629, -20.46040770435011069, 31.16992750791695599 ) ) ;
#8344 = CARTESIAN_POINT ( 'NONE',  ( -2.500000000000001776, 64.00000000000000000, 49.30000000218494449 ) ) ;
#8345 = ORIENTED_EDGE ( 'NONE', *, *, #15528, .T. ) ;
#8346 = CARTESIAN_POINT ( 'NONE',  ( -18.78091578003892081, -20.46040770435013556, 31.83007249208304401 ) ) ;
#8347 = VECTOR ( 'NONE', #7878, 1000.000000000000000 ) ;
#8348 = AXIS2_PLACEMENT_3D ( 'NONE', #16990, #6685, #3450 ) ;
#8349 = DIRECTION ( 'NONE',  ( -1.000000000000000000, 0.000000000000000000, 0.000000000000000000 ) ) ;
#8350 = VERTEX_POINT ( 'NONE', #4579 ) ;
#8351 = CARTESIAN_POINT ( 'NONE',  ( -11.95583473709190514, -24.63902057219072361, 28.76757249208304401 ) ) ;
#8352 = CARTESIAN_POINT ( 'NONE',  ( -15.00000000000000000, 47.00000000000000711, 30.00000000000000000 ) ) ;
#8353 = ORIENTED_EDGE ( 'NONE', *, *, #9166, .F. ) ;
#8354 = CARTESIAN_POINT ( 'NONE',  ( 1.300000000000000044, 1.478016689125442484, -1.626303258728256651E-15 ) ) ;
#8355 = ORIENTED_EDGE ( 'NONE', *, *, #4473, .F. ) ;
#8356 = EDGE_CURVE ( 'NONE', #5200, #15466, #9449, .T. ) ;
#8357 = DIRECTION ( 'NONE',  ( 0.000000000000000000, 0.000000000000000000, 1.000000000000000000 ) ) ;
#8358 = DIRECTION ( 'NONE',  ( -1.000000000000000000, 0.000000000000000000, -1.541976423090495633E-16 ) ) ;
#8359 = CARTESIAN_POINT ( 'NONE',  ( 1.767766952966370653, 62.23223304703363112, 48.00000000218494023 ) ) ;
#8360 = AXIS2_PLACEMENT_3D ( 'NONE', #10173, #9010, #18045 ) ;
#8361 = PLANE ( 'NONE',  #3888 ) ;
#8362 = EDGE_CURVE ( 'NONE', #12628, #16874, #18404, .T. ) ;
#8363 = CARTESIAN_POINT ( 'NONE',  ( -41.00000000000000711, 110.0000000000000000, 27.50000000000000000 ) ) ;
#8364 = DIRECTION ( 'NONE',  ( 0.000000000000000000, -1.000000000000000000, 0.000000000000000000 ) ) ;
#8365 = PLANE ( 'NONE',  #8642 ) ;
#8366 = VERTEX_POINT ( 'NONE', #5069 ) ;
#8367 = ORIENTED_EDGE ( 'NONE', *, *, #15020, .F. ) ;
#8368 = CARTESIAN_POINT ( 'NONE',  ( -10.58745947852649927, -21.64274437364853654, 31.38867750791696309 ) ) ;
#8369 = CARTESIAN_POINT ( 'NONE',  ( 1.461580736456473684, 65.46158073645646880, 48.45000000109247651 ) ) ;
#8370 = CARTESIAN_POINT ( 'NONE',  ( -9.955834737091903364, -25.17491895705294880, 28.76757249208304401 ) ) ;
#8371 = DIRECTION ( 'NONE',  ( -0.000000000000000000, 0.7071067811865456854, 0.7071067811865494601 ) ) ;
#8372 = DIRECTION ( 'NONE',  ( 0.000000000000000000, 0.000000000000000000, 1.000000000000000000 ) ) ;
#8373 = EDGE_CURVE ( 'NONE', #763, #10477, #6326, .T. ) ;
#8374 = CARTESIAN_POINT ( 'NONE',  ( -19.99999999999999645, -23.83517299489738051, 29.20117750791695599 ) ) ;
#8375 = FACE_OUTER_BOUND ( 'NONE', #12145, .T. ) ;
#8376 = CARTESIAN_POINT ( 'NONE',  ( -19.24771351637089367, -21.35725562635142438, 29.63867750791695599 ) ) ;
#8377 = CARTESIAN_POINT ( 'NONE',  ( -15.16482700510263371, -18.99999999999997868, 21.98632249208304401 ) ) ;
#8378 = CARTESIAN_POINT ( 'NONE',  ( 1.767766952966370653, 62.23223304703363112, 49.49999999999999289 ) ) ;
#8379 = DIRECTION ( 'NONE',  ( 1.000000000000000000, -0.000000000000000000, -0.000000000000000000 ) ) ;
#8380 = CARTESIAN_POINT ( 'NONE',  ( -31.74999999999995737, 0.000000000000000000, 2.750000000000000000 ) ) ;
#8381 = CARTESIAN_POINT ( 'NONE',  ( 2.500000000000001776, 65.03553390593273775, 49.64999999999999147 ) ) ;
#8382 = CARTESIAN_POINT ( 'NONE',  ( 0.2500000000000002220, 0.000000000000000000, 4.250000000000000000 ) ) ;
#8383 = VERTEX_POINT ( 'NONE', #18103 ) ;
#8384 = LINE ( 'NONE', #14356, #4053 ) ;
#8385 = CARTESIAN_POINT ( 'NONE',  ( -17.68048971390461688, -25.35725562635141372, 39.26367750791696665 ) ) ;
#8386 = FACE_OUTER_BOUND ( 'NONE', #10408, .T. ) ;
#8387 = CARTESIAN_POINT ( 'NONE',  ( -8.044165262908093084, -21.95952864787946979, 33.58007249208304046 ) ) ;
#8388 = CARTESIAN_POINT ( 'NONE',  ( -0.8561741729129461742, 66.06698729999999387, 44.60000000109246088 ) ) ;
#8389 = ORIENTED_EDGE ( 'NONE', *, *, #16510, .F. ) ;
#8390 = LINE ( 'NONE', #9573, #8163 ) ;
#8391 = DIRECTION ( 'NONE',  ( 1.000000000000000000, 0.000000000000000000, 2.973811673103096679E-16 ) ) ;
#8392 = CARTESIAN_POINT ( 'NONE',  ( -0.8561741729129461742, 66.06698730000000808, 47.80000000109247082 ) ) ;
#8393 = DIRECTION ( 'NONE',  ( -1.000000000000000000, -0.000000000000000000, -0.000000000000000000 ) ) ;
#8394 = EDGE_CURVE ( 'NONE', #2269, #12927, #6534, .T. ) ;
#8395 = EDGE_CURVE ( 'NONE', #13503, #10710, #452, .T. ) ;
#8396 = VECTOR ( 'NONE', #10535, 1000.000000000000000 ) ;
#8397 = CARTESIAN_POINT ( 'NONE',  ( 0.000000000000000000, 1.478016689125442484, -1.626303258728256651E-15 ) ) ;
#8398 = EDGE_CURVE ( 'NONE', #13986, #10157, #16928, .T. ) ;
#8399 = DIRECTION ( 'NONE',  ( 1.000000000000000000, 0.000000000000000000, 2.973811673103096679E-16 ) ) ;
#8400 = ORIENTED_EDGE ( 'NONE', *, *, #15721, .F. ) ;
#8401 = ORIENTED_EDGE ( 'NONE', *, *, #6076, .T. ) ;
#8402 = CARTESIAN_POINT ( 'NONE',  ( -17.04047135212050890, -17.04416526290807710, 6.017572492083039570 ) ) ;
#8403 = EDGE_CURVE ( 'NONE', #14706, #10838, #994, .T. ) ;
#8404 = VERTEX_POINT ( 'NONE', #12206 ) ;
#8406 = ORIENTED_EDGE ( 'NONE', *, *, #510, .F. ) ;
#8405 = EDGE_LOOP ( 'NONE', ( #17338, #15835 ) ) ;
#8407 = CARTESIAN_POINT ( 'NONE',  ( -13.64274437364856141, -26.68048971390460622, 1.201177507916959986 ) ) ;
#8408 = CARTESIAN_POINT ( 'NONE',  ( -21.95583473709191580, -21.95952864787954084, 29.41992750791695954 ) ) ;
#8409 = CIRCLE ( 'NONE', #10913, 10.00000000000000178 ) ;
#8410 = CARTESIAN_POINT ( 'NONE',  ( 44.99999999999998579, 3.000000000000000000, -54.99999999999998579 ) ) ;
#8411 = CARTESIAN_POINT ( 'NONE',  ( -1.035533905932738863, 61.50000000000000000, 47.85000000218494165 ) ) ;
#8412 = CARTESIAN_POINT ( 'NONE',  ( 43.49999999999997868, 2.999000000000001442, -52.50000000000002132 ) ) ;
#8413 = ORIENTED_EDGE ( 'NONE', *, *, #7687, .T. ) ;
#8414 = EDGE_CURVE ( 'NONE', #18580, #7844, #9361, .T. ) ;
#8415 = DIRECTION ( 'NONE',  ( 0.000000000000000000, 0.000000000000000000, 1.000000000000000000 ) ) ;
#8416 = ORIENTED_EDGE ( 'NONE', *, *, #8395, .T. ) ;
#8417 = DIRECTION ( 'NONE',  ( -0.000000000000000000, -0.7071067811865493491, 0.7071067811865456854 ) ) ;
#8418 = ORIENTED_EDGE ( 'NONE', *, *, #18190, .T. ) ;
#8419 = DIRECTION ( 'NONE',  ( 1.000000000000000000, -0.000000000000000000, -0.000000000000000000 ) ) ;
#8420 = DIRECTION ( 'NONE',  ( 0.000000000000000000, 0.000000000000000000, -1.000000000000000000 ) ) ;
#8421 = CARTESIAN_POINT ( 'NONE',  ( -32.50000000000000000, 53.00000000000000711, -37.64999999999999858 ) ) ;
#8422 = VECTOR ( 'NONE', #14278, 1000.000000000000000 ) ;
#8423 = CARTESIAN_POINT ( 'NONE',  ( -0.8561741729129465073, 61.93301270000000613, 45.70000000109248361 ) ) ;
#8424 = EDGE_CURVE ( 'NONE', #9017, #12139, #18222, .T. ) ;
#8425 = FACE_OUTER_BOUND ( 'NONE', #15230, .T. ) ;
#8426 = CARTESIAN_POINT ( 'NONE',  ( -2.500000000000001776, 64.00000000000000000, 49.99999999999999289 ) ) ;
#8427 = CARTESIAN_POINT ( 'NONE',  ( 1.609560293423944355, 62.54174113348394570, 45.00000000000002132 ) ) ;
#8428 = ORIENTED_EDGE ( 'NONE', *, *, #44, .F. ) ;
#8429 = ORIENTED_EDGE ( 'NONE', *, *, #423, .T. ) ;
#8430 = CARTESIAN_POINT ( 'NONE',  ( -9.020235676060220698, -27.64274437364852588, 6.013677507916956877 ) ) ;
#8431 = LINE ( 'NONE', #17269, #4622 ) ;
#8432 = VERTEX_POINT ( 'NONE', #15451 ) ;
#8433 = CARTESIAN_POINT ( 'NONE',  ( -12.04416526290808420, -23.03132541760398766, 7.330072492083044011 ) ) ;
#8434 = AXIS2_PLACEMENT_3D ( 'NONE', #10508, #17676, #1611 ) ;
#8435 = EDGE_CURVE ( 'NONE', #9439, #3017, #2018, .T. ) ;
#8436 = EDGE_CURVE ( 'NONE', #5657, #16384, #8008, .T. ) ;
#8437 = CARTESIAN_POINT ( 'NONE',  ( 2.500000000000000000, -1.178949249685218970, -2.041999999999998039 ) ) ;
#8438 = APPLICATION_CONTEXT ( 'automotive_design' ) ;
#8439 = ORIENTED_EDGE ( 'NONE', *, *, #11905, .F. ) ;
#8440 = CARTESIAN_POINT ( 'NONE',  ( -15.96867458239599635, -21.04416526290806999, 27.01757249208303691 ) ) ;
#8441 = VECTOR ( 'NONE', #730, 1000.000000000000000 ) ;
#8442 = DIRECTION ( 'NONE',  ( 0.000000000000000000, 0.000000000000000000, -1.000000000000000000 ) ) ;
#8443 = ORIENTED_EDGE ( 'NONE', *, *, #15327, .F. ) ;
#8444 = VECTOR ( 'NONE', #9294, 1000.000000000000000 ) ;
#8445 = CARTESIAN_POINT ( 'NONE',  ( -40.00000000000000000, 52.00000000000000711, 30.00000000000000000 ) ) ;
#8446 = ORIENTED_EDGE ( 'NONE', *, *, #8504, .T. ) ;
#8447 = DIRECTION ( 'NONE',  ( 0.000000000000000000, -1.000000000000000000, 0.000000000000000000 ) ) ;
#8448 = ADVANCED_FACE ( 'NONE', ( #18500 ), #18208, .F. ) ;
#8449 = LINE ( 'NONE', #14618, #8009 ) ;
#8450 = CARTESIAN_POINT ( 'NONE',  ( 2.500000000000001776, 64.00000000000000000, 48.10000000218494165 ) ) ;
#8451 = VECTOR ( 'NONE', #432, 1000.000000000000000 ) ;
#8452 = CARTESIAN_POINT ( 'NONE',  ( -13.49542703274178379, -19.04416526290806289, 25.48242750791694888 ) ) ;
#8453 = AXIS2_PLACEMENT_3D ( 'NONE', #6651, #9850, #15846 ) ;
#8454 = FACE_OUTER_BOUND ( 'NONE', #2407, .T. ) ;
#8455 = CARTESIAN_POINT ( 'NONE',  ( -13.49542703274178379, -19.04416526290806289, -0.7675724920830416798 ) ) ;
#8456 = VECTOR ( 'NONE', #1061, 1000.000000000000114 ) ;
#8457 = LINE ( 'NONE', #7671, #14594 ) ;
#8458 = VERTEX_POINT ( 'NONE', #13877 ) ;
#8459 = EDGE_CURVE ( 'NONE', #16384, #14710, #7710, .T. ) ;
#8460 = CARTESIAN_POINT ( 'NONE',  ( -9.020235676060250896, -20.35725562635137820, 28.11132249208304046 ) ) ;
#8461 = CARTESIAN_POINT ( 'NONE',  ( -10.75228648362910100, -26.64274437364854009, 37.51367750791695954 ) ) ;
#8462 = CARTESIAN_POINT ( 'NONE',  ( 2.066987300000001859, 64.85617417291294373, 47.60000000109246798 ) ) ;
#8463 = CARTESIAN_POINT ( 'NONE',  ( -17.64274437364858983, -19.75228648362910633, 32.04882249208304046 ) ) ;
#8464 = CARTESIAN_POINT ( 'NONE',  ( -0.8561741729129461742, 66.06698729999999387, 44.60000000109246088 ) ) ;
#8465 = VECTOR ( 'NONE', #10314, 1000.000000000000000 ) ;
#8466 = PLANE ( 'NONE',  #15012 ) ;
#8467 = CARTESIAN_POINT ( 'NONE',  ( -17.35725562635144215, -19.58745947852648683, 35.32617750791695954 ) ) ;
#8468 = CARTESIAN_POINT ( 'NONE',  ( -44.99999999999998579, 0.000000000000000000, -56.59999999999999432 ) ) ;
#8469 = CARTESIAN_POINT ( 'NONE',  ( -10.04416526290807710, -25.50457296725819489, 32.04492750791695954 ) ) ;
#8470 = AXIS2_PLACEMENT_3D ( 'NONE', #4510, #13705, #10370 ) ;
#8471 = CARTESIAN_POINT ( 'NONE',  ( -15.00000000000001421, -18.99999999999997868, -4.336808689942017736E-16 ) ) ;
#8472 = CARTESIAN_POINT ( 'NONE',  ( -12.64274437364858628, -19.58745947852646552, 38.17382249208304046 ) ) ;
#8473 = CARTESIAN_POINT ( 'NONE',  ( 1.461580736456473906, 62.53841926354353120, 45.25000000109247367 ) ) ;
#8474 = CARTESIAN_POINT ( 'NONE',  ( 1.461580736456473906, 62.53841926354353120, 49.25000000109246656 ) ) ;
#8475 = VECTOR ( 'NONE', #4426, 1000.000000000000000 ) ;
#8476 = DIRECTION ( 'NONE',  ( 0.000000000000000000, 0.000000000000000000, 1.000000000000000000 ) ) ;
#8477 = CARTESIAN_POINT ( 'NONE',  ( 3.796994071234847710E-16, 61.93301269999999903, 45.15000000109247225 ) ) ;
#8478 = DIRECTION ( 'NONE',  ( 0.000000000000000000, -1.000000000000000000, 0.000000000000000000 ) ) ;
#8479 = AXIS2_PLACEMENT_3D ( 'NONE', #12850, #7165, #14425 ) ;
#8480 = ORIENTED_EDGE ( 'NONE', *, *, #15119, .T. ) ;
#8481 = VECTOR ( 'NONE', #2236, 1000.000000000000227 ) ;
#8482 = CARTESIAN_POINT ( 'NONE',  ( 0.8561741729129460632, 66.06698730000000808, 46.10000000109246798 ) ) ;
#8483 = CARTESIAN_POINT ( 'NONE',  ( -16.17491895705301275, -18.95583473709189803, 4.044927507916959541 ) ) ;
#8484 = CARTESIAN_POINT ( 'NONE',  ( -25.00000000000000000, 53.00000000000000711, -5.000000000000004441 ) ) ;
#8485 = CARTESIAN_POINT ( 'NONE',  ( -9.996306089212408708, -18.75498260482328661, 33.14257249208303335 ) ) ;
#8486 = CARTESIAN_POINT ( 'NONE',  ( 2.066987300000001859, 64.85617417291294373, 49.40000000109246514 ) ) ;
#8487 = ORIENTED_EDGE ( 'NONE', *, *, #625, .T. ) ;
#8488 = DIRECTION ( 'NONE',  ( -1.000000000000000000, -0.000000000000000000, -0.000000000000000000 ) ) ;
#8489 = DIRECTION ( 'NONE',  ( 0.000000000000000000, 1.000000000000000000, -1.471414886128461669E-15 ) ) ;
#8490 = VECTOR ( 'NONE', #14922, 1000.000000000000000 ) ;
#8491 = CARTESIAN_POINT ( 'NONE',  ( -0.8561741729129466183, 61.93301270000000613, 47.30000000109247082 ) ) ;
#8492 = LINE ( 'NONE', #5553, #9991 ) ;
#8493 = VECTOR ( 'NONE', #13105, 1000.000000000000000 ) ;
#8494 = PLANE ( 'NONE',  #6934 ) ;
#8495 = DIRECTION ( 'NONE',  ( 1.000000000000000000, -0.000000000000000000, -0.000000000000000000 ) ) ;
#8496 = CARTESIAN_POINT ( 'NONE',  ( 1.767766952966370653, 62.23223304703363112, 47.89999999999999858 ) ) ;
#8497 = ORIENTED_EDGE ( 'NONE', *, *, #13961, .T. ) ;
#8498 = ORIENTED_EDGE ( 'NONE', *, *, #13564, .F. ) ;
#8499 = CARTESIAN_POINT ( 'NONE',  ( -20.97976432393974022, -27.64274437364858628, 4.486322492083039570 ) ) ;
#8500 = ORIENTED_EDGE ( 'NONE', *, *, #9457, .T. ) ;
#8502 = ORIENTED_EDGE ( 'NONE', *, *, #17427, .T. ) ;
#8501 = ORIENTED_EDGE ( 'NONE', *, *, #654, .F. ) ;
#8503 = CARTESIAN_POINT ( 'NONE',  ( -17.99999999999999645, -23.83517299489736985, 8.201177507916959541 ) ) ;
#8504 = EDGE_CURVE ( 'NONE', #6374, #10710, #6438, .T. ) ;
#8505 = CARTESIAN_POINT ( 'NONE',  ( -14.83517299489740715, -16.99999999999997868, 35.76367750791694533 ) ) ;
#8506 = VECTOR ( 'NONE', #15960, 1000.000000000000000 ) ;
#8507 = DIRECTION ( 'NONE',  ( -0.000000000000000000, -0.000000000000000000, -1.000000000000000000 ) ) ;
#8508 = CARTESIAN_POINT ( 'NONE',  ( -1.530808498934192803E-16, 66.50000000000000000, 46.70000000218494307 ) ) ;
#8509 = CARTESIAN_POINT ( 'NONE',  ( 0.000000000000000000, 0.000000000000000000, 30.00000000000000000 ) ) ;
#8510 = ORIENTED_EDGE ( 'NONE', *, *, #4900, .F. ) ;
#8511 = ADVANCED_FACE ( 'NONE', ( #11025 ), #17027, .T. ) ;
#8512 = DIRECTION ( 'NONE',  ( -0.000000000000000000, -0.000000000000000000, -1.000000000000000000 ) ) ;
#8513 = ORIENTED_EDGE ( 'NONE', *, *, #11880, .T. ) ;
#8514 = LINE ( 'NONE', #15590, #8456 ) ;
#8515 = EDGE_LOOP ( 'NONE', ( #6209, #18236, #3923, #6362 ) ) ;
#8516 = LINE ( 'NONE', #7138, #8493 ) ;
#8517 = CARTESIAN_POINT ( 'NONE',  ( -12.70357423236093197, -43.78611686177728046, 3.000000000000000000 ) ) ;
#8518 = DIRECTION ( 'NONE',  ( -0.000000000000000000, -1.000000000000000000, 0.000000000000000000 ) ) ;
#8519 = EDGE_CURVE ( 'NONE', #1447, #7718, #15549, .T. ) ;
#8520 = CARTESIAN_POINT ( 'NONE',  ( 2.066987300000001859, 64.85617417291294373, 46.00000000109246656 ) ) ;
#8521 = FACE_OUTER_BOUND ( 'NONE', #8341, .T. ) ;
#8522 = SHAPE_REPRESENTATION ( 'socket head cap screw_iso_ISO 4762 M3 x 8 - 8N', ( #1791 ), #1419 ) ;
#8523 = CARTESIAN_POINT ( 'NONE',  ( -41.00000000000000711, 53.00000000000000711, 13.50000000000000000 ) ) ;
#8524 = CARTESIAN_POINT ( 'NONE',  ( 0.7910017786515960436, 62.09035273295529578, 44.99999999999998579 ) ) ;
#8525 = ORIENTED_EDGE ( 'NONE', *, *, #2677, .F. ) ;
#8527 = VERTEX_POINT ( 'NONE', #644 ) ;
#8526 = ORIENTED_EDGE ( 'NONE', *, *, #13942, .F. ) ;
#8528 = CARTESIAN_POINT ( 'NONE',  ( -7.999999999999996447, -24.16482700510256976, 0.3261775079169564884 ) ) ;
#8529 = DIRECTION ( 'NONE',  ( 1.000000000000000000, -0.000000000000000000, -0.000000000000000000 ) ) ;
#8530 = ORIENTED_EDGE ( 'NONE', *, *, #10533, .F. ) ;
#8531 = CIRCLE ( 'NONE', #18575, 2.499999999999998668 ) ;
#8532 = CARTESIAN_POINT ( 'NONE',  ( -15.63902057219073605, -27.04416526290807710, 3.830072492083042679 ) ) ;
#8533 = EDGE_CURVE ( 'NONE', #10285, #1200, #10632, .T. ) ;
#8534 = CARTESIAN_POINT ( 'NONE',  ( 2.500000000000002220, 62.96446609406726935, 45.54999999999999716 ) ) ;
#8535 = EDGE_LOOP ( 'NONE', ( #15089, #10470, #19378, #14176 ) ) ;
#8536 = CARTESIAN_POINT ( 'NONE',  ( -12.48433729119798130, -25.64274437364855075, 6.013677507916959541 ) ) ;
#8537 = CARTESIAN_POINT ( 'NONE',  ( -41.00000000000000711, 53.00000000000000711, 1.500000000000001332 ) ) ;
#8538 = ORIENTED_EDGE ( 'NONE', *, *, #4989, .T. ) ;
#8539 = CARTESIAN_POINT ( 'NONE',  ( -50.00000000000001421, 0.000000000000000000, 59.99999999999997868 ) ) ;
#8540 = EDGE_LOOP ( 'NONE', ( #5172, #13853, #2332, #9108 ) ) ;
#8541 = LINE ( 'NONE', #896, #322 ) ;
#8542 = PLANE ( 'NONE',  #15520 ) ;
#8543 = CARTESIAN_POINT ( 'NONE',  ( -1.040834085586084257E-14, 32.57106781186547551, 49.67157287525382969 ) ) ;
#8544 = DIRECTION ( 'NONE',  ( 1.156482317317871725E-16, 0.000000000000000000, -1.000000000000000000 ) ) ;
#8545 = ADVANCED_FACE ( 'NONE', ( #9175 ), #15160, .T. ) ;
#8546 = CARTESIAN_POINT ( 'NONE',  ( -19.41254052147348830, -26.35725562635142083, 34.01367750791696665 ) ) ;
#8547 = ADVANCED_FACE ( 'NONE', ( #5711 ), #6718, .T. ) ;
#8548 = CARTESIAN_POINT ( 'NONE',  ( -41.00000000000000711, 53.00000000000000711, 21.00000000000000000 ) ) ;
#8549 = EDGE_CURVE ( 'NONE', #10801, #6744, #15640, .T. ) ;
#8550 = CARTESIAN_POINT ( 'NONE',  ( -9.999999999999994671, -24.16482700510257686, 0.3261775079169582647 ) ) ;
#8551 = DIRECTION ( 'NONE',  ( 1.000000000000000000, -0.000000000000000000, -0.000000000000000000 ) ) ;
#8552 = ORIENTED_EDGE ( 'NONE', *, *, #1109, .F. ) ;
#8553 = CARTESIAN_POINT ( 'NONE',  ( -10.75228648362912232, -21.35725562635138530, 1.861322492083040903 ) ) ;
#8554 = CARTESIAN_POINT ( 'NONE',  ( -19.95583473709191580, -22.49542703274176603, 39.91992750791695954 ) ) ;
#8555 = CARTESIAN_POINT ( 'NONE',  ( 2.066987300000001859, 64.85617417291294373, 48.40000000109247225 ) ) ;
#8556 = CARTESIAN_POINT ( 'NONE',  ( -11.46040770435014977, -20.21908421996103655, 27.89257249208303335 ) ) ;
#8557 = PLANE ( 'NONE',  #15674 ) ;
#8558 = ORIENTED_EDGE ( 'NONE', *, *, #15200, .F. ) ;
#8559 = CARTESIAN_POINT ( 'NONE',  ( -18.78091578003889950, -27.53959229564985378, 33.79492750791696665 ) ) ;
#8560 = LINE ( 'NONE', #12963, #17060 ) ;
#8561 = CARTESIAN_POINT ( 'NONE',  ( -8.528048594804062077, -45.28611686177728046, 3.000000000000000000 ) ) ;
#8562 = FACE_OUTER_BOUND ( 'NONE', #8040, .T. ) ;
#8563 = CARTESIAN_POINT ( 'NONE',  ( -11.46040770435015332, -20.21908421996104011, 33.14257249208303335 ) ) ;
#8564 = EDGE_CURVE ( 'NONE', #297, #13006, #11121, .T. ) ;
#8565 = EDGE_CURVE ( 'NONE', #16200, #16449, #11568, .T. ) ;
#8566 = CARTESIAN_POINT ( 'NONE',  ( -2.500000000000001776, 64.00000000000000000, 47.59999999999999432 ) ) ;
#8567 = CARTESIAN_POINT ( 'NONE',  ( -1.767766952966369765, 62.23223304703363112, 49.29999999999999716 ) ) ;
#8568 = CARTESIAN_POINT ( 'NONE',  ( 24.00000000000000000, 52.00000000000000711, -67.72004514666936359 ) ) ;
#8569 = CARTESIAN_POINT ( 'NONE',  ( -2.500000000000001776, 65.03553390593273775, 49.14999999999999858 ) ) ;
#8570 = CARTESIAN_POINT ( 'NONE',  ( 4.130991513055717768, 26.86292658466335936, 59.62172003681460808 ) ) ;
#8571 = ORIENTED_EDGE ( 'NONE', *, *, #1582, .F. ) ;
#8572 =( NAMED_UNIT ( * ) PLANE_ANGLE_UNIT ( ) SI_UNIT ( $, .RADIAN. ) );
#8573 = CARTESIAN_POINT ( 'NONE',  ( -2.066987300000001415, 64.85617417291294373, 44.70000000109248361 ) ) ;
#8574 = AXIS2_PLACEMENT_3D ( 'NONE', #6323, #339, #6515 ) ;
#8575 = CARTESIAN_POINT ( 'NONE',  ( -16.50457296725820555, -28.95583473709189448, 7.107427507916955989 ) ) ;
#8576 = CARTESIAN_POINT ( 'NONE',  ( -4.000000000000001776, 67.00000000000000000, 34.99999999999999289 ) ) ;
#8577 = CARTESIAN_POINT ( 'NONE',  ( -22.04416526290809486, -22.28918265808477628, 36.64257249208304046 ) ) ;
#8578 = CARTESIAN_POINT ( 'NONE',  ( 0.8561741729129472844, 61.93301270000000613, 49.20000000109247651 ) ) ;
#8579 = CARTESIAN_POINT ( 'NONE',  ( -17.99999999999999645, -23.83517299489736985, 34.45117750791695954 ) ) ;
#8580 = CARTESIAN_POINT ( 'NONE',  ( -16.50457296725820555, -28.95583473709189803, 7.107427507916956877 ) ) ;
#8581 = LINE ( 'NONE', #14657, #13826 ) ;
#8582 = EDGE_CURVE ( 'NONE', #2908, #17921, #7167, .T. ) ;
#8583 = CARTESIAN_POINT ( 'NONE',  ( 1.461580736456473906, 62.53841926354353120, 46.65000000109247225 ) ) ;
#8584 = LINE ( 'NONE', #1137, #16228 ) ;
#8585 =( GEOMETRIC_REPRESENTATION_CONTEXT ( 3 ) GLOBAL_UNCERTAINTY_ASSIGNED_CONTEXT ( ( #9037 ) ) GLOBAL_UNIT_ASSIGNED_CONTEXT ( ( #653, #1031, #7005 ) ) REPRESENTATION_CONTEXT ( 'NONE', 'WORKASPACE' ) );
#8586 = PLANE ( 'NONE',  #13183 ) ;
#8587 = VECTOR ( 'NONE', #2987, 1000.000000000000000 ) ;
#8588 = CARTESIAN_POINT ( 'NONE',  ( -2.500000000000001776, 64.00000000000000000, 48.39999999999999858 ) ) ;
#8589 = DIRECTION ( 'NONE',  ( 3.826732013112564095E-16, -1.000000000000000000, -1.632680918566406793E-16 ) ) ;
#8590 = ORIENTED_EDGE ( 'NONE', *, *, #5392, .F. ) ;
#8591 = ORIENTED_EDGE ( 'NONE', *, *, #17392, .T. ) ;
#8592 = CARTESIAN_POINT ( 'NONE',  ( -20.97976432393974022, -27.64274437364858628, 9.736322492083036906 ) ) ;
#8593 = ORIENTED_EDGE ( 'NONE', *, *, #3737, .T. ) ;
#8595 = VERTEX_POINT ( 'NONE', #17659 ) ;
#8594 = VERTEX_POINT ( 'NONE', #12688 ) ;
#8596 = CARTESIAN_POINT ( 'NONE',  ( -17.68048971390461688, -25.35725562635141372, 2.513677507916959986 ) ) ;
#8597 = CARTESIAN_POINT ( 'NONE',  ( -18.35725562635144925, -17.85540867095761186, 35.32617750791695244 ) ) ;
#8598 = AXIS2_PLACEMENT_3D ( 'NONE', #9060, #16716, #15336 ) ;
#8599 = VECTOR ( 'NONE', #7866, 1000.000000000000000 ) ;
#8600 = CARTESIAN_POINT ( 'NONE',  ( 2.492551403682577771, 31.38014068711926541, 55.10514068711930236 ) ) ;
#8601 = CARTESIAN_POINT ( 'NONE',  ( -1.035533905932738641, 66.50000000000000000, 45.95000000218494307 ) ) ;
#8602 = DIRECTION ( 'NONE',  ( 0.000000000000000000, -1.000000000000000000, -0.000000000000000000 ) ) ;
#8603 = ORIENTED_EDGE ( 'NONE', *, *, #2569, .F. ) ;
#8604 = CARTESIAN_POINT ( 'NONE',  ( -41.00000000000000711, 53.00000000000000711, -32.00000000000000000 ) ) ;
#8605 = ORIENTED_EDGE ( 'NONE', *, *, #4457, .F. ) ;
#8606 = PLANE ( 'NONE',  #15973 ) ;
#8607 = ORIENTED_EDGE ( 'NONE', *, *, #18100, .T. ) ;
#8608 = LINE ( 'NONE', #11252, #6926 ) ;
#8609 = LINE ( 'NONE', #1162, #2467 ) ;
#8610 = DIRECTION ( 'NONE',  ( -0.000000000000000000, 1.000000000000000000, -0.000000000000000000 ) ) ;
#8611 = CARTESIAN_POINT ( 'NONE',  ( 2.066987300000001859, 64.85617417291294373, 49.40000000109246514 ) ) ;
#8612 = DIRECTION ( 'NONE',  ( 0.000000000000000000, 0.000000000000000000, -1.000000000000000000 ) ) ;
#8613 = AXIS2_PLACEMENT_3D ( 'NONE', #8039, #7744, #572 ) ;
#8614 = CARTESIAN_POINT ( 'NONE',  ( 12.99999999999999822, 0.000000000000000000, 0.000000000000000000 ) ) ;
#8615 = AXIS2_PLACEMENT_3D ( 'NONE', #1644, #15357, #12210 ) ;
#8616 = CARTESIAN_POINT ( 'NONE',  ( 50.00000000000000000, 33.00000000000000000, 59.99999999999997868 ) ) ;
#8617 = ORIENTED_EDGE ( 'NONE', *, *, #3495, .T. ) ;
#8619 = ORIENTED_EDGE ( 'NONE', *, *, #14769, .F. ) ;
#8618 = VERTEX_POINT ( 'NONE', #1297 ) ;
#8620 = CARTESIAN_POINT ( 'NONE',  ( -22.04416526290807710, -25.71081734191525925, 2.732427507916957321 ) ) ;
#8621 = CARTESIAN_POINT ( 'NONE',  ( -41.00000000000000711, 110.0000000000000000, 20.00000000000000000 ) ) ;
#8622 = EDGE_LOOP ( 'NONE', ( #14812, #14683, #17946, #1371 ) ) ;
#8623 = CARTESIAN_POINT ( 'NONE',  ( -16.50457296725825174, -19.04416526290807354, 42.76757249208303335 ) ) ;
#8624 = DIRECTION ( 'NONE',  ( -0.000000000000000000, -0.000000000000000000, -1.000000000000000000 ) ) ;
#8625 = ORIENTED_EDGE ( 'NONE', *, *, #9608, .F. ) ;
#8626 = CARTESIAN_POINT ( 'NONE',  ( -17.68048971390462754, -22.64274437364856496, 42.11132249208304756 ) ) ;
#8627 = AXIS2_PLACEMENT_3D ( 'NONE', #5656, #11619, #7415 ) ;
#8628 = PLANE ( 'NONE',  #8788 ) ;
#8629 = VERTEX_POINT ( 'NONE', #16186 ) ;
#8630 = VECTOR ( 'NONE', #6122, 1000.000000000000000 ) ;
#8631 = CARTESIAN_POINT ( 'NONE',  ( -25.00000000000000000, 53.00000000000000711, 30.00000000000000000 ) ) ;
#8632 = ORIENTED_EDGE ( 'NONE', *, *, #5937, .T. ) ;
#8633 = CARTESIAN_POINT ( 'NONE',  ( -41.00000000000000711, 53.00000000000000711, 13.50000000000000000 ) ) ;
#8634 = DIRECTION ( 'NONE',  ( -2.775557561562890858E-16, 0.7071067811865454633, 0.7071067811865496822 ) ) ;
#8635 = LINE ( 'NONE', #5709, #15064 ) ;
#8636 = DIRECTION ( 'NONE',  ( -7.709882115452476934E-17, -0.000000000000000000, -1.000000000000000000 ) ) ;
#8637 = ADVANCED_FACE ( 'NONE', ( #5802 ), #2754, .T. ) ;
#8638 = ADVANCED_FACE ( 'NONE', ( #16088 ), #5507, .T. ) ;
#8639 = CARTESIAN_POINT ( 'NONE',  ( -10.58745947852649927, -21.64274437364853654, 26.13867750791695599 ) ) ;
#8640 = FACE_BOUND ( 'NONE', #5573, .T. ) ;
#8641 = CARTESIAN_POINT ( 'NONE',  ( -11.21908421996108629, -20.46040770435011069, -0.3300724920830416798 ) ) ;
#8642 = AXIS2_PLACEMENT_3D ( 'NONE', #17572, #4149, #13042 ) ;
#8643 = CARTESIAN_POINT ( 'NONE',  ( -15.16482700510263371, -18.99999999999997868, 42.98632249208304046 ) ) ;
#8644 = VERTEX_POINT ( 'NONE', #14621 ) ;
#8645 = AXIS2_PLACEMENT_3D ( 'NONE', #15415, #115, #16785 ) ;
#8646 = CARTESIAN_POINT ( 'NONE',  ( -8.855408670957602979, -27.35725562635137820, 39.48632249208304046 ) ) ;
#8647 = CARTESIAN_POINT ( 'NONE',  ( -19.99999999999999645, -23.83517299489738051, 39.70117750791695954 ) ) ;
#8648 = CARTESIAN_POINT ( 'NONE',  ( 0.8561741729129472844, 61.93301270000000613, 48.20000000109248361 ) ) ;
#8649 = CARTESIAN_POINT ( 'NONE',  ( -16.64274437364858272, -21.48433729119797420, 5.798822492083043123 ) ) ;
#8650 = LINE ( 'NONE', #14341, #9092 ) ;
#8651 = ORIENTED_EDGE ( 'NONE', *, *, #2594, .F. ) ;
#8652 = EDGE_CURVE ( 'NONE', #12114, #3704, #14764, .T. ) ;
#8653 = CARTESIAN_POINT ( 'NONE',  ( 1.300000000000000044, 1.108512516844080364, -0.6400000000000017897 ) ) ;
#8654 = CARTESIAN_POINT ( 'NONE',  ( -6.528048594804060301, -45.28611686177728046, 1.500000000000000000 ) ) ;
#8655 = EDGE_CURVE ( 'NONE', #8882, #2308, #11669, .T. ) ;
#8656 = DIRECTION ( 'NONE',  ( 8.163404592832032733E-17, 0.000000000000000000, 1.000000000000000000 ) ) ;
#8657 = CARTESIAN_POINT ( 'NONE',  ( -19.24771351637089367, -21.35725562635142438, 40.13867750791695954 ) ) ;
#8658 = DIRECTION ( 'NONE',  ( 0.000000000000000000, 0.7071067811865456854, 0.7071067811865494601 ) ) ;
#8659 = CARTESIAN_POINT ( 'NONE',  ( -16.50457296725825174, -19.04416526290807354, 32.26757249208304046 ) ) ;
#8660 = AXIS2_PLACEMENT_3D ( 'NONE', #4168, #10119, #13167 ) ;
#8661 = CARTESIAN_POINT ( 'NONE',  ( -2.500000000000001776, 65.03553390593273775, 46.74999999999999289 ) ) ;
#8662 = CARTESIAN_POINT ( 'NONE',  ( -0.8561741729129461742, 66.06698730000000808, 48.80000000109247082 ) ) ;
#8663 = CARTESIAN_POINT ( 'NONE',  ( 2.499999999999996003, 62.96446609406726225, 48.85000000218494165 ) ) ;
#8664 = CARTESIAN_POINT ( 'NONE',  ( 2.500000000000001776, 64.00000000000000000, 46.39999999999999858 ) ) ;
#8665 = LINE ( 'NONE', #7395, #9580 ) ;
#8666 = ORIENTED_EDGE ( 'NONE', *, *, #11548, .T. ) ;
#8667 = CARTESIAN_POINT ( 'NONE',  ( -11.21908421996108629, -20.46040770435011069, 10.16992750791695244 ) ) ;
#8668 = CARTESIAN_POINT ( 'NONE',  ( -11.21908421996108629, -20.46040770435011069, -0.3300724920830416798 ) ) ;
#8669 = LINE ( 'NONE', #18976, #6650 ) ;
#8670 = CARTESIAN_POINT ( 'NONE',  ( -14.83517299489735741, -28.99999999999998224, 8.861322492083040459 ) ) ;
#8671 = EDGE_CURVE ( 'NONE', #5010, #9208, #11470, .T. ) ;
#8672 = CARTESIAN_POINT ( 'NONE',  ( 0.8561741729129460632, 66.06698729999999387, 49.50000000109246656 ) ) ;
#8673 = CARTESIAN_POINT ( 'NONE',  ( -12.68318583509884157, -21.92450931948787485, 36.41992750791695954 ) ) ;
#8674 = CARTESIAN_POINT ( 'NONE',  ( -13.82508104294698015, -29.04416526290806289, 1.419927507916958209 ) ) ;
#8675 = LINE ( 'NONE', #14366, #6322 ) ;
#8676 = EDGE_CURVE ( 'NONE', #8045, #15565, #5159, .T. ) ;
#8677 = CARTESIAN_POINT ( 'NONE',  ( 32.50000000000000000, -6.000000000000000000, -42.49999999999999289 ) ) ;
#8678 = FACE_OUTER_BOUND ( 'NONE', #6198, .T. ) ;
#8679 = LINE ( 'NONE', #1436, #2865 ) ;
#8680 = DIRECTION ( 'NONE',  ( 0.000000000000000000, -0.6139406135149195753, 0.7893522173763268812 ) ) ;
#8681 = CARTESIAN_POINT ( 'NONE',  ( 50.00000000000000000, 6.000000000000005329, -56.99999999999999289 ) ) ;
#8682 = LINE ( 'NONE', #13085, #10513 ) ;
#8683 = ORIENTED_EDGE ( 'NONE', *, *, #15071, .F. ) ;
#8684 = ORIENTED_EDGE ( 'NONE', *, *, #6199, .F. ) ;
#8685 = CARTESIAN_POINT ( 'NONE',  ( -20.24501739517669563, -18.99630608921239627, 5.580072492083037794 ) ) ;
#8686 = ORIENTED_EDGE ( 'NONE', *, *, #2698, .F. ) ;
#8687 = CARTESIAN_POINT ( 'NONE',  ( -10.04416526290808598, -22.49542703274172695, 2.080072492083040903 ) ) ;
#8689 = ORIENTED_EDGE ( 'NONE', *, *, #16826, .T. ) ;
#8688 = ORIENTED_EDGE ( 'NONE', *, *, #988, .T. ) ;
#8690 = EDGE_CURVE ( 'NONE', #18230, #5758, #8728, .T. ) ;
#8691 = CARTESIAN_POINT ( 'NONE',  ( -12.68318583509884157, -21.92450931948787485, -0.3300724920830400699 ) ) ;
#8692 = CARTESIAN_POINT ( 'NONE',  ( -11.35725562635144925, -18.02023567606020293, 25.70117750791695599 ) ) ;
#8693 = DIRECTION ( 'NONE',  ( -1.000000000000000000, -3.826732013112563602E-16, 0.000000000000000000 ) ) ;
#8694 = CARTESIAN_POINT ( 'NONE',  ( -0.8561741729129461742, 66.06698729999999387, 49.40000000109247225 ) ) ;
#8695 = CARTESIAN_POINT ( 'NONE',  ( 12.55500000000001748, 3.061616997868383634E-16, -2.500000000000000444 ) ) ;
#8696 = ORIENTED_EDGE ( 'NONE', *, *, #280, .T. ) ;
#8697 = PLANE ( 'NONE',  #4410 ) ;
#8698 = EDGE_LOOP ( 'NONE', ( #12013, #3994, #10460, #14002 ) ) ;
#8699 = ORIENTED_EDGE ( 'NONE', *, *, #3546, .T. ) ;
#8700 = PLANE ( 'NONE',  #13520 ) ;
#8701 = CARTESIAN_POINT ( 'NONE',  ( -41.00000000000000711, 53.00000000000000711, -38.50000000000000711 ) ) ;
#8702 = CARTESIAN_POINT ( 'NONE',  ( -7.499999999999994671, -26.00000000000000355, 12.50000000000000000 ) ) ;
#8703 = CARTESIAN_POINT ( 'NONE',  ( 1.461580736456473906, 62.53841926354353120, 49.25000000109246656 ) ) ;
#8704 = DIRECTION ( 'NONE',  ( 0.000000000000000000, 0.000000000000000000, 1.000000000000000000 ) ) ;
#8705 = CARTESIAN_POINT ( 'NONE',  ( -7.499999999999994671, -38.00000000000000000, 4.500000000000000888 ) ) ;
#8706 = LINE ( 'NONE', #8815, #16128 ) ;
#8707 = VERTEX_POINT ( 'NONE', #13037 ) ;
#8709 = ORIENTED_EDGE ( 'NONE', *, *, #12707, .T. ) ;
#8708 = EDGE_LOOP ( 'NONE', ( #17104, #19251 ) ) ;
#8710 = CARTESIAN_POINT ( 'NONE',  ( -20.97976432393977575, -20.35725562635143504, 3.388677507916956877 ) ) ;
#8711 = VECTOR ( 'NONE', #8006, 1000.000000000000000 ) ;
#8712 = CARTESIAN_POINT ( 'NONE',  ( -1.767766952966370209, 65.76776695296638309, 45.09999999999999432 ) ) ;
#8713 = ORIENTED_EDGE ( 'NONE', *, *, #5580, .T. ) ;
#8714 = ORIENTED_EDGE ( 'NONE', *, *, #11090, .T. ) ;
#8715 = CARTESIAN_POINT ( 'NONE',  ( -18.53959229564982536, -27.78091578003890660, 41.01757249208304046 ) ) ;
#8716 = LINE ( 'NONE', #4320, #15023 ) ;
#8717 = ORIENTED_EDGE ( 'NONE', *, *, #2186, .F. ) ;
#8718 = CARTESIAN_POINT ( 'NONE',  ( -15.63902057219076269, -20.95583473709189448, 4.044927507916962206 ) ) ;
#8719 = VECTOR ( 'NONE', #12659, 1000.000000000000000 ) ;
#8720 = LINE ( 'NONE', #2944, #1603 ) ;
#8721 = ORIENTED_EDGE ( 'NONE', *, *, #1701, .T. ) ;
#8722 = DIRECTION ( 'NONE',  ( -1.000000000000000000, 0.000000000000000000, 0.000000000000000000 ) ) ;
#8723 = ORIENTED_EDGE ( 'NONE', *, *, #2292, .T. ) ;
#8724 = LINE ( 'NONE', #16183, #19120 ) ;
#8725 = CARTESIAN_POINT ( 'NONE',  ( 3.399999999999998135, 29.83102903476756751, 56.65425233947098604 ) ) ;
#8726 = VECTOR ( 'NONE', #3195, 1000.000000000000000 ) ;
#8727 = CARTESIAN_POINT ( 'NONE',  ( -1.265664690411616068E-16, 66.06698730000000808, 44.55000000109247082 ) ) ;
#8728 = LINE ( 'NONE', #17118, #14436 ) ;
#8729 = CARTESIAN_POINT ( 'NONE',  ( -13.82508104294698192, -29.04416526290806644, 32.91992750791695954 ) ) ;
#8730 = CYLINDRICAL_SURFACE ( 'NONE', #11736, 4.000000000000001776 ) ;
#8731 = LINE ( 'NONE', #5904, #3652 ) ;
#8732 = AXIS2_PLACEMENT_3D ( 'NONE', #13854, #6510, #13751 ) ;
#8733 = DIRECTION ( 'NONE',  ( -1.000000000000000000, 0.000000000000000000, 0.000000000000000000 ) ) ;
#8734 = VERTEX_POINT ( 'NONE', #14718 ) ;
#8735 = CARTESIAN_POINT ( 'NONE',  ( -10.04416526290808953, -22.49542703274172695, 2.080072492083040903 ) ) ;
#8736 = VECTOR ( 'NONE', #11000, 1000.000000000000000 ) ;
#8737 = CARTESIAN_POINT ( 'NONE',  ( -9.754982604823348780, -18.99630608921234654, 10.16992750791695777 ) ) ;
#8738 = VECTOR ( 'NONE', #4807, 1000.000000000000000 ) ;
#8739 = CARTESIAN_POINT ( 'NONE',  ( -2.066987300000001415, 63.14382582708705627, 45.60000000109246088 ) ) ;
#8740 = EDGE_CURVE ( 'NONE', #14902, #17473, #17461, .T. ) ;
#8741 = EDGE_CURVE ( 'NONE', #13505, #6660, #9999, .T. ) ;
#8742 = CARTESIAN_POINT ( 'NONE',  ( -12.04416526290808420, -23.03132541760398766, 2.080072492083043567 ) ) ;
#8743 = FACE_OUTER_BOUND ( 'NONE', #7358, .T. ) ;
#8744 = VERTEX_POINT ( 'NONE', #14823 ) ;
#8745 = VECTOR ( 'NONE', #3817, 1000.000000000000000 ) ;
#8746 = CARTESIAN_POINT ( 'NONE',  ( -10.20349328142095224, -22.14960319667834909, 2.322403871605816721E-12 ) ) ;
#8747 = DIRECTION ( 'NONE',  ( 1.000000000000000000, 0.000000000000000000, 0.000000000000000000 ) ) ;
#8748 = EDGE_CURVE ( 'NONE', #6376, #16061, #16900, .T. ) ;
#8749 = CARTESIAN_POINT ( 'NONE',  ( 44.99999999999998579, 3.000000000000000000, -54.99999999999998579 ) ) ;
#8750 = CARTESIAN_POINT ( 'NONE',  ( -24.00000000000000000, 110.0000000000000000, -5.999999999999998224 ) ) ;
#8751 = CARTESIAN_POINT ( 'NONE',  ( -3.155775640247338920, -38.39960408384397539, 3.000000000000000000 ) ) ;
#8752 = CARTESIAN_POINT ( 'NONE',  ( -17.35725562635140307, -28.41254052147349185, 40.79882249208304046 ) ) ;
#8753 = CARTESIAN_POINT ( 'NONE',  ( -1.767766952966370209, 65.76776695296638309, 47.49999999999999289 ) ) ;
#8754 = CARTESIAN_POINT ( 'NONE',  ( -0.8561741729129461742, 66.06698730000000808, 48.00000000109246656 ) ) ;
#8755 = EDGE_CURVE ( 'NONE', #9977, #2631, #6099, .T. ) ;
#8756 = AXIS2_PLACEMENT_3D ( 'NONE', #13533, #6093, #10584 ) ;
#8757 = CARTESIAN_POINT ( 'NONE',  ( -1.767766952966370209, 65.76776695296638309, 46.69999999999999574 ) ) ;
#8758 = CARTESIAN_POINT ( 'NONE',  ( 2.500000000000001776, 64.00000000000000000, 45.59999999999999432 ) ) ;
#8759 = LINE ( 'NONE', #16029, #4903 ) ;
#8760 = AXIS2_PLACEMENT_3D ( 'NONE', #3342, #15682, #2252 ) ;
#8761 = ORIENTED_EDGE ( 'NONE', *, *, #4338, .T. ) ;
#8762 = EDGE_CURVE ( 'NONE', #17252, #9239, #15117, .T. ) ;
#8763 = SURFACE_STYLE_USAGE ( .BOTH. , #7199 ) ;
#8764 = CARTESIAN_POINT ( 'NONE',  ( -9.955834737091912245, -22.82508104294696594, 0.1074275079169582509 ) ) ;
#8765 = CARTESIAN_POINT ( 'NONE',  ( -11.46040770435012668, -27.78091578003887463, 11.48242750791695954 ) ) ;
#8766 = CARTESIAN_POINT ( 'NONE',  ( -1.035533905932738641, 66.50000000000000000, 48.35000000218494165 ) ) ;
#8767 = CARTESIAN_POINT ( 'NONE',  ( -12.64274437364858628, -19.58745947852646552, 11.92382249208304223 ) ) ;
#8768 = AXIS2_PLACEMENT_3D ( 'NONE', #6953, #3124, #14245 ) ;
#8769 = CARTESIAN_POINT ( 'NONE',  ( -1.461580736456473462, 62.53841926354353120, 49.05000000109247082 ) ) ;
#8770 = CARTESIAN_POINT ( 'NONE',  ( -9.999999999999994671, -24.16482700510257686, 5.576177507916958653 ) ) ;
#8771 = CARTESIAN_POINT ( 'NONE',  ( -14.83517299489739649, -18.99999999999997868, 9.513677507916957765 ) ) ;
#8772 = CARTESIAN_POINT ( 'NONE',  ( -2.500000000000001776, 64.00000000000000000, 49.30000000218494449 ) ) ;
#8773 = CARTESIAN_POINT ( 'NONE',  ( -1.265664690411616068E-16, 66.06698730000000808, 49.55000000109247082 ) ) ;
#8774 = CARTESIAN_POINT ( 'NONE',  ( -10.00000000000000000, 0.000000000000000000, 1.500000000000000444 ) ) ;
#8775 = CARTESIAN_POINT ( 'NONE',  ( 0.000000000000000000, -32.00000000000000711, 1.500000000000000000 ) ) ;
#8776 = AXIS2_PLACEMENT_3D ( 'NONE', #13753, #3072, #16805 ) ;
#8777 = CARTESIAN_POINT ( 'NONE',  ( 0.8561741729129460632, 66.06698730000000808, 46.30000000109247082 ) ) ;
#8778 = DIRECTION ( 'NONE',  ( 0.000000000000000000, 0.000000000000000000, 1.000000000000000000 ) ) ;
#8779 = VECTOR ( 'NONE', #17505, 1000.000000000000000 ) ;
#8780 = EDGE_CURVE ( 'NONE', #1682, #14847, #15525, .T. ) ;
#8781 = ADVANCED_FACE ( 'NONE', ( #3253 ), #5900, .F. ) ;
#8782 = CARTESIAN_POINT ( 'NONE',  ( 0.1249999999999895917, 25.46464466094064250, 60.66708332270462734 ) ) ;
#8783 = ORIENTED_EDGE ( 'NONE', *, *, #16958, .T. ) ;
#8784 = VERTEX_POINT ( 'NONE', #9133 ) ;
#8785 = EDGE_CURVE ( 'NONE', #2835, #2239, #1786, .T. ) ;
#8786 = CARTESIAN_POINT ( 'NONE',  ( -7.999999999999996447, -23.83517299489733432, 18.04882249208304046 ) ) ;
#8787 = FILL_AREA_STYLE_COLOUR ( '', #13681 ) ;
#8788 = AXIS2_PLACEMENT_3D ( 'NONE', #7158, #15801, #14709 ) ;
#8789 = CARTESIAN_POINT ( 'NONE',  ( -2.500000000000001776, 64.00000000000000000, 47.59999999999999432 ) ) ;
#8791 = ORIENTED_EDGE ( 'NONE', *, *, #13703, .T. ) ;
#8790 = ORIENTED_EDGE ( 'NONE', *, *, #10869, .T. ) ;
#8792 = PRODUCT_DEFINITION_SHAPE ( 'NONE', 'NONE',  #6693 ) ;
#8793 = CARTESIAN_POINT ( 'NONE',  ( -15.63902057219073605, -27.04416526290807710, 40.58007249208304756 ) ) ;
#8794 = EDGE_CURVE ( 'NONE', #16792, #3171, #6014, .T. ) ;
#8795 = DIRECTION ( 'NONE',  ( 1.000000000000000000, 0.000000000000000000, 0.000000000000000000 ) ) ;
#8796 = CARTESIAN_POINT ( 'NONE',  ( -18.35725562635144925, -17.85540867095761186, 40.57617750791695244 ) ) ;
#8797 = VECTOR ( 'NONE', #3250, 1000.000000000000000 ) ;
#8798 = LINE ( 'NONE', #3904, #8506 ) ;
#8799 = CARTESIAN_POINT ( 'NONE',  ( 1.461580736456473684, 65.46158073645646880, 48.45000000109247651 ) ) ;
#8800 = ORIENTED_EDGE ( 'NONE', *, *, #8676, .F. ) ;
#8801 = ORIENTED_EDGE ( 'NONE', *, *, #2786, .F. ) ;
#8802 = AXIS2_PLACEMENT_3D ( 'NONE', #19105, #13009, #872 ) ;
#8803 = ORIENTED_EDGE ( 'NONE', *, *, #9256, .T. ) ;
#8804 = VERTEX_POINT ( 'NONE', #4833 ) ;
#8805 = CARTESIAN_POINT ( 'NONE',  ( -10.00000000000000000, 0.000000000000000000, 7.499999999999995559 ) ) ;
#8806 = LINE ( 'NONE', #8701, #15632 ) ;
#8807 = DIRECTION ( 'NONE',  ( 0.000000000000000000, 1.000000000000000000, 0.000000000000000000 ) ) ;
#8808 = AXIS2_PLACEMENT_3D ( 'NONE', #15470, #2409, #6922 ) ;
#8809 = CARTESIAN_POINT ( 'NONE',  ( -0.8561741729129461742, 66.06698729999999387, 47.20000000109247651 ) ) ;
#8810 = ADVANCED_FACE ( 'NONE', ( #17962 ), #1391, .T. ) ;
#8811 = EDGE_CURVE ( 'NONE', #1380, #19125, #15016, .T. ) ;
#8812 = FACE_OUTER_BOUND ( 'NONE', #3929, .T. ) ;
#8813 = VECTOR ( 'NONE', #6634, 1000.000000000000000 ) ;
#8814 = B_SPLINE_CURVE_WITH_KNOTS ( 'NONE', 3,
 ( #989, #6965, #12840, #17451 ),
 .UNSPECIFIED., .F., .F.,
 ( 4, 4 ),
 ( 0.000000000000000000, 1.000000000000000000 ),
 .UNSPECIFIED. ) ;
#8815 = CARTESIAN_POINT ( 'NONE',  ( -35.00000000000002132, -0.000000000000000000, -47.50000000000002132 ) ) ;
#8816 = ORIENTED_EDGE ( 'NONE', *, *, #18058, .F. ) ;
#8818 = ORIENTED_EDGE ( 'NONE', *, *, #2099, .T. ) ;
#8817 = ORIENTED_EDGE ( 'NONE', *, *, #15174, .F. ) ;
#8819 = CARTESIAN_POINT ( 'NONE',  ( -17.04047135212043784, -30.95583473709190159, 1.857427507916956211 ) ) ;
#8820 = CIRCLE ( 'NONE', #11316, 1.500000000000001332 ) ;
#8821 = CARTESIAN_POINT ( 'NONE',  ( -37.50000000000002132, -6.000000000000000000, -25.00000000000002132 ) ) ;
#8822 = ORIENTED_EDGE ( 'NONE', *, *, #16910, .T. ) ;
#8823 = ORIENTED_EDGE ( 'NONE', *, *, #6285, .F. ) ;
#8824 = CARTESIAN_POINT ( 'NONE',  ( -14.36097942780925685, -20.95583473709189093, 6.455072492083044899 ) ) ;
#8825 = CARTESIAN_POINT ( 'NONE',  ( -50.00000000000002132, 33.00000000000000000, 44.99999999999999289 ) ) ;
#8826 = DIRECTION ( 'NONE',  ( 1.000000000000000000, 0.000000000000000000, 2.081668171172167774E-16 ) ) ;
#8827 = ORIENTED_EDGE ( 'NONE', *, *, #3395, .T. ) ;
#8828 = CARTESIAN_POINT ( 'NONE',  ( -12.68318583509884157, -21.92450931948787485, 4.919927507916961318 ) ) ;
#8829 = DIRECTION ( 'NONE',  ( 0.000000000000000000, -0.5000000000000011102, -0.8660254037844379305 ) ) ;
#8830 = ORIENTED_EDGE ( 'NONE', *, *, #18890, .F. ) ;
#8831 = DIRECTION ( 'NONE',  ( -0.000000000000000000, -0.000000000000000000, -1.000000000000000000 ) ) ;
#8832 = ORIENTED_EDGE ( 'NONE', *, *, #14412, .T. ) ;
#8833 = CARTESIAN_POINT ( 'NONE',  ( -24.00000000000000711, 53.00000000000000711, -25.50000000000000000 ) ) ;
#8834 = CARTESIAN_POINT ( 'NONE',  ( -15.00000000000000000, 0.000000000000000000, 0.000000000000000000 ) ) ;
#8835 = PLANE ( 'NONE',  #18523 ) ;
#8836 = EDGE_CURVE ( 'NONE', #13043, #3590, #12161, .T. ) ;
#8837 = DIRECTION ( 'NONE',  ( -0.000000000000000000, -0.000000000000000000, -1.000000000000000000 ) ) ;
#8838 = CARTESIAN_POINT ( 'NONE',  ( -19.95583473709191580, -22.49542703274176603, 29.41992750791695599 ) ) ;
#8839 = AXIS2_PLACEMENT_3D ( 'NONE', #4403, #10365, #16358 ) ;
#8840 = CARTESIAN_POINT ( 'NONE',  ( -4.189607678530337331, 26.72836399182265055, 59.40336399182262284 ) ) ;
#8841 = DIRECTION ( 'NONE',  ( 0.000000000000000000, 1.000000000000000000, -9.912705577010328508E-16 ) ) ;
#8842 = ORIENTED_EDGE ( 'NONE', *, *, #11284, .F. ) ;
#8843 = PRODUCT_DEFINITION_CONTEXT ( 'detailed design', #13441, 'design' ) ;
#8844 = CARTESIAN_POINT ( 'NONE',  ( -9.955834737091903364, -25.17491895705294880, 2.517572492083040903 ) ) ;
#8845 = CARTESIAN_POINT ( 'NONE',  ( -17.35725562635144215, -19.58745947852648683, 40.57617750791696665 ) ) ;
#8846 = CARTESIAN_POINT ( 'NONE',  ( -24.00000000000000000, 110.0000000000000000, -32.00000000000000000 ) ) ;
#8847 = CARTESIAN_POINT ( 'NONE',  ( -14.03132541760400009, -26.95583473709189448, 8.642572492083042235 ) ) ;
#8848 = DIRECTION ( 'NONE',  ( 0.000000000000000000, 0.000000000000000000, 1.000000000000000000 ) ) ;
#8849 = ORIENTED_EDGE ( 'NONE', *, *, #15513, .T. ) ;
#8850 = CARTESIAN_POINT ( 'NONE',  ( -24.00000000000000000, 110.0000000000000000, -12.49999999999999645 ) ) ;
#8851 = VERTEX_POINT ( 'NONE', #1592 ) ;
#8852 = CARTESIAN_POINT ( 'NONE',  ( -50.00000000000002132, 0.000000000000000000, -60.00000000000002132 ) ) ;
#8853 = DIRECTION ( 'NONE',  ( -7.304098846218135653E-17, 0.000000000000000000, 1.000000000000000000 ) ) ;
#8854 = CARTESIAN_POINT ( 'NONE',  ( 2.500000000000001776, 65.03553390593273775, 44.95000000218495018 ) ) ;
#8855 = DIRECTION ( 'NONE',  ( 1.000000000000000000, -0.000000000000000000, -0.000000000000000000 ) ) ;
#8856 = DIRECTION ( 'NONE',  ( -1.000000000000000000, 0.000000000000000000, -0.000000000000000000 ) ) ;
#8857 = CARTESIAN_POINT ( 'NONE',  ( -1.530808498934192803E-16, 66.50000000000000000, 48.19999999999999574 ) ) ;
#8858 = CARTESIAN_POINT ( 'NONE',  ( -1.265664690411616068E-16, 66.06698730000000808, 47.95000000109246940 ) ) ;
#8859 = DIRECTION ( 'NONE',  ( 2.220446049250313081E-16, 0.7071067811865452413, 0.7071067811865497932 ) ) ;
#8860 = CARTESIAN_POINT ( 'NONE',  ( -2.500000000000001776, 65.03553390593273775, 46.74999999999999289 ) ) ;
#8861 = DIRECTION ( 'NONE',  ( 0.000000000000000000, 0.000000000000000000, -1.000000000000000000 ) ) ;
#8862 = ORIENTED_EDGE ( 'NONE', *, *, #4967, .T. ) ;
#8863 =( BOUNDED_SURFACE ( )  B_SPLINE_SURFACE ( 1, 2, ( 
 ( #13077, #1533, #19175, #15061, #8773, #16426, #8972, #14959, #1825, #18498, #12204, #10629, #9358, #3582, #3298, #7804, #9268, #156, #15254, #17025, #1726, #18402, #450, #13974, #13776, #6436, #16729, #1928, #12307, #16632, #18303, #356, #6342, #9554, #5067, #12497, #4968, #1638, #546, #6144, #16926, #2016, #4871, #6531, #10832, #7910, #11023, #16827, #8005, #3389, #6238, #15349, #7611, #15449, #18206, #13875, #4782, #12404, #3199, #10925, #3488, #13575, #9173, #15158, #7708, #12104, #9463, #18101, #10733, #4673, #13674, #253, #5157, #5347, #15826, #17116, #14069, #9833, #5441, #18590, #17390, #642, #12878, #2209, #6904, #8101, #737, #15740, #6632, #5534, #8473, #6716, #18963, #921, #8286, #18877, #12967, #15922, #17480, #11492, #12599 ),
 ( #17211, #4058, #11118, #3965, #6999, #15637, #3679, #17305, #15547, #11309, #8378, #9748, #6811, #3867, #12777, #11396, #12686, #2393, #11206, #2484, #3778, #14348, #18690, #9650, #5254, #14449, #18772, #9924, #1025, #8202, #14168, #2302, #2117, #14256, #829, #17681, #8857, #19056, #7189, #13060, #5629, #2776, #7096, #4166, #4359, #13259, #1320, #10116, #8566, #2879, #8753, #7292, #14544, #16115, #14742, #16025, #4259, #2680, #19257, #5825, #11591, #10023, #11791, #14842, #17589, #8661, #17783, #14641, #10315, #2584, #1115, #13163, #7388, #1414, #1208, #19160, #5731, #11690, #10220, #16209, #16311, #5496, #15708, #11364, #12933, #11273, #8166, #5227, #4022, #8534, #2364, #14508, #6692, #1079, #7057, #5409, #2276, #11181, #9898, #13028, #11554 ) ),
 .UNSPECIFIED., .F., .F., .F. ) 
 B_SPLINE_SURFACE_WITH_KNOTS ( ( 2, 2 ),
 ( 3, 2, 2, 2, 2, 2, 2, 2, 2, 2, 2, 2, 2, 2, 2, 2, 2, 2, 2, 2, 2, 2, 2, 2, 2, 2, 2, 2, 2, 2, 2, 2, 2, 2, 2, 2, 2, 2, 2, 2, 2, 2, 2, 2, 2, 2, 2, 2, 2, 2, 3 ),
 ( 0.000000000000000000, 1.000000000000000000 ),
 ( 0.000000000000000000, 0.01785714285714285615, 0.03571428571428571230, 0.05357142857142856845, 0.07142857142857142461, 0.08928571428571428770, 0.1071428571428571369, 0.1250000000000000000, 0.1428571428571428492, 0.1607142857142857262, 0.1785714285714285754, 0.1964285714285714246, 0.2142857142857142738, 0.2321428571428571508, 0.2500000000000000000, 0.2678571428571428492, 0.2857142857142856984, 0.3035714285714285476, 0.3214285714285714524, 0.3392857142857143016, 0.3571428571428571508, 0.3750000000000000000, 0.3928571428571428492, 0.4107142857142856984, 0.4285714285714285476, 0.4464285714285714524, 0.4642857142857143016, 0.4821428571428571508, 0.5000000000000000000, 0.5178571428571429047, 0.5357142857142856984, 0.5535714285714286031, 0.5714285714285713969, 0.5892857142857143016, 0.6071428571428570953, 0.6250000000000000000, 0.6428571428571429047, 0.6607142857142856984, 0.6785714285714286031, 0.6964285714285713969, 0.7142857142857143016, 0.7321428571428570953, 0.7500000000000000000, 0.7678571428571429047, 0.7857142857142856984, 0.8035714285714286031, 0.8214285714285713969, 0.8392857142857143016, 0.8571428571428570953, 0.8750000000000000000, 0.8928571428571429047 ),
 .UNSPECIFIED. ) 
 GEOMETRIC_REPRESENTATION_ITEM ( )  RATIONAL_B_SPLINE_SURFACE ( (
 ( 1.000000000000000000, 0.9238795325112867385, 1.000000000000000000, 0.9238795325112867385, 1.000000000000000000, 0.9238795325112867385, 1.000000000000000000, 0.9238795325112867385, 1.000000000000000000, 0.9238795325112867385, 1.000000000000000000, 0.9238795325112867385, 1.000000000000000000, 0.9238795325112867385, 1.000000000000000000, 0.9238795325112867385, 1.000000000000000000, 0.9238795325112867385, 1.000000000000000000, 0.9238795325112867385, 1.000000000000000000, 0.9238795325112867385, 1.000000000000000000, 0.9238795325112867385, 1.000000000000000000, 0.9238795325112867385, 1.000000000000000000, 0.9238795325112867385, 1.000000000000000000, 0.9238795325112867385, 1.000000000000000000, 0.9238795325112867385, 1.000000000000000000, 0.9238795325112867385, 1.000000000000000000, 0.9238795325112867385, 1.000000000000000000, 0.9238795325112867385, 1.000000000000000000, 0.9238795325112867385, 1.000000000000000000, 0.9238795325112867385, 1.000000000000000000, 0.9238795325112867385, 1.000000000000000000, 0.9238795325112867385, 1.000000000000000000, 0.9238795325112867385, 1.000000000000000000, 0.9238795325112867385, 1.000000000000000000, 0.9238795325112867385, 1.000000000000000000, 0.9238795325112867385, 1.000000000000000000, 0.9238795325112867385, 1.000000000000000000, 0.9238795325112867385, 1.000000000000000000, 0.9238795325112867385, 1.000000000000000000, 0.9238795325112867385, 1.000000000000000000, 0.9238795325112867385, 1.000000000000000000, 0.9238795325112867385, 1.000000000000000000, 0.9238795325112867385, 1.000000000000000000, 0.9238795325112867385, 1.000000000000000000, 0.9238795325112867385, 1.000000000000000000, 0.9238795325112867385, 1.000000000000000000, 0.9238795325112867385, 1.000000000000000000, 0.9238795325112867385, 1.000000000000000000, 0.9238795325112867385, 1.000000000000000000, 0.9238795325112867385, 1.000000000000000000, 0.9238795325112867385, 1.000000000000000000, 0.9238795325112867385, 1.000000000000000000, 0.9238795325112867385, 1.000000000000000000, 0.9238795325112867385, 1.000000000000000000, 0.9238795325112867385, 1.000000000000000000, 0.9238795325112867385, 1.000000000000000000, 0.9238795325112867385, 1.000000000000000000, 0.9238795325112867385, 1.000000000000000000, 0.9238795325112867385, 1.000000000000000000),
 ( 1.000000000000000000, 0.9238795325112867385, 1.000000000000000000, 0.9238795325112867385, 1.000000000000000000, 0.9238795325112867385, 1.000000000000000000, 0.9238795325112867385, 1.000000000000000000, 0.9238795325112867385, 1.000000000000000000, 0.9238795325112867385, 1.000000000000000000, 0.9238795325112867385, 1.000000000000000000, 0.9238795325112867385, 1.000000000000000000, 0.9238795325112867385, 1.000000000000000000, 0.9238795325112867385, 1.000000000000000000, 0.9238795325112867385, 1.000000000000000000, 0.9238795325112867385, 1.000000000000000000, 0.9238795325112867385, 1.000000000000000000, 0.9238795325112867385, 1.000000000000000000, 0.9238795325112867385, 1.000000000000000000, 0.9238795325112867385, 1.000000000000000000, 0.9238795325112867385, 1.000000000000000000, 0.9238795325112867385, 1.000000000000000000, 0.9238795325112867385, 1.000000000000000000, 0.9238795325112867385, 1.000000000000000000, 0.9238795325112867385, 1.000000000000000000, 0.9238795325112867385, 1.000000000000000000, 0.9238795325112867385, 1.000000000000000000, 0.9238795325112867385, 1.000000000000000000, 0.9238795325112867385, 1.000000000000000000, 0.9238795325112867385, 1.000000000000000000, 0.9238795325112867385, 1.000000000000000000, 0.9238795325112867385, 1.000000000000000000, 0.9238795325112867385, 1.000000000000000000, 0.9238795325112867385, 1.000000000000000000, 0.9238795325112867385, 1.000000000000000000, 0.9238795325112867385, 1.000000000000000000, 0.9238795325112867385, 1.000000000000000000, 0.9238795325112867385, 1.000000000000000000, 0.9238795325112867385, 1.000000000000000000, 0.9238795325112867385, 1.000000000000000000, 0.9238795325112867385, 1.000000000000000000, 0.9238795325112867385, 1.000000000000000000, 0.9238795325112867385, 1.000000000000000000, 0.9238795325112867385, 1.000000000000000000, 0.9238795325112867385, 1.000000000000000000, 0.9238795325112867385, 1.000000000000000000, 0.9238795325112867385, 1.000000000000000000, 0.9238795325112867385, 1.000000000000000000, 0.9238795325112867385, 1.000000000000000000, 0.9238795325112867385, 1.000000000000000000, 0.9238795325112867385, 1.000000000000000000, 0.9238795325112867385, 1.000000000000000000, 0.9238795325112867385, 1.000000000000000000, 0.9238795325112867385, 1.000000000000000000) ) ) 
 REPRESENTATION_ITEM ( '' )  SURFACE ( )  );
#8864 = DIRECTION ( 'NONE',  ( 1.000000000000000000, 0.000000000000000000, 0.000000000000000000 ) ) ;
#8865 = CARTESIAN_POINT ( 'NONE',  ( -19.41254052147348830, -26.35725562635142083, 7.763677507916958653 ) ) ;
#8866 = CARTESIAN_POINT ( 'NONE',  ( -19.95583473709191580, -22.49542703274176603, 18.91992750791694888 ) ) ;
#8867 = CARTESIAN_POINT ( 'NONE',  ( -1.530808498934192803E-16, 66.50000000000000000, 49.10000000218494165 ) ) ;
#8868 = CARTESIAN_POINT ( 'NONE',  ( -12.35725562635140307, -28.24771351637085459, 8.423822492083042235 ) ) ;
#8869 = CARTESIAN_POINT ( 'NONE',  ( -2.066987300000001859, 64.85617417291294373, 46.50000000109246656 ) ) ;
#8870 = CARTESIAN_POINT ( 'NONE',  ( -19.24771351637089367, -21.35725562635142438, 8.638677507916957765 ) ) ;
#8871 = EDGE_CURVE ( 'NONE', #18238, #8707, #7565, .T. ) ;
#8872 = CARTESIAN_POINT ( 'NONE',  ( -12.64274437364855252, -28.41254052147347053, 6.451177507916959541 ) ) ;
#8873 = FACE_OUTER_BOUND ( 'NONE', #2382, .T. ) ;
#8874 = LINE ( 'NONE', #17605, #6561 ) ;
#8875 = FACE_OUTER_BOUND ( 'NONE', #15949, .T. ) ;
#8876 = CARTESIAN_POINT ( 'NONE',  ( 2.500000000000001776, 64.00000000000000000, 49.60000000000000142 ) ) ;
#8877 = FACE_OUTER_BOUND ( 'NONE', #3558, .T. ) ;
#8878 = CARTESIAN_POINT ( 'NONE',  ( -32.50000000000000000, 52.00000000000000711, -35.00000000000000000 ) ) ;
#8879 = EDGE_CURVE ( 'NONE', #13949, #3613, #9028, .T. ) ;
#8880 = DIRECTION ( 'NONE',  ( 0.000000000000000000, 0.000000000000000000, -1.000000000000000000 ) ) ;
#8881 = ORIENTED_EDGE ( 'NONE', *, *, #12064, .T. ) ;
#8882 = VERTEX_POINT ( 'NONE', #10590 ) ;
#8883 = CARTESIAN_POINT ( 'NONE',  ( -9.754982604823302594, -29.00369391078756465, 23.95507249208304046 ) ) ;
#8884 = SURFACE_STYLE_FILL_AREA ( #1544 ) ;
#8885 = DIRECTION ( 'NONE',  ( 0.000000000000000000, 0.000000000000000000, 1.000000000000000000 ) ) ;
#8887 = ORIENTED_EDGE ( 'NONE', *, *, #4222, .T. ) ;
#8886 = VERTEX_POINT ( 'NONE', #4736 ) ;
#8888 = CARTESIAN_POINT ( 'NONE',  ( -12.68318583509884157, -21.92450931948787485, 15.41992750791695954 ) ) ;
#8889 = PLANE ( 'NONE',  #19275 ) ;
#8890 = CARTESIAN_POINT ( 'NONE',  ( -21.95583473709191580, -21.95952864787954084, 39.91992750791695954 ) ) ;
#8891 = CARTESIAN_POINT ( 'NONE',  ( 2.066987300000001415, 64.00000000000000000, 49.15000000109247225 ) ) ;
#8892 = CARTESIAN_POINT ( 'NONE',  ( -1.035533905932738641, 66.50000000000000000, 45.15000000218493881 ) ) ;
#8893 = ORIENTED_EDGE ( 'NONE', *, *, #276, .F. ) ;
#8894 = ORIENTED_EDGE ( 'NONE', *, *, #15756, .T. ) ;
#8895 = CARTESIAN_POINT ( 'NONE',  ( 4.012354697599916697, 26.78000129688588871, 59.70432772728319293 ) ) ;
#8896 = CARTESIAN_POINT ( 'NONE',  ( 41.99999999999998579, 139.6861997365471950, -52.00000000000000000 ) ) ;
#8897 = EDGE_CURVE ( 'NONE', #2845, #18598, #18161, .T. ) ;
#8898 = EDGE_CURVE ( 'NONE', #18807, #14701, #15218, .T. ) ;
#8899 = CIRCLE ( 'NONE', #7651, 2.500000000000002220 ) ;
#8900 = EDGE_LOOP ( 'NONE', ( #19185, #10269, #3512, #12152 ) ) ;
#8901 = DIRECTION ( 'NONE',  ( 1.000000000000000000, 0.000000000000000000, 0.000000000000000000 ) ) ;
#8902 = DIRECTION ( 'NONE',  ( 1.000000000000000000, -0.000000000000000000, -0.000000000000000000 ) ) ;
#8903 = EDGE_CURVE ( 'NONE', #14415, #18998, #18264, .T. ) ;
#8904 = CARTESIAN_POINT ( 'NONE',  ( -1.461580736456473906, 65.46158073645646880, 48.85000000109246798 ) ) ;
#8905 = CARTESIAN_POINT ( 'NONE',  ( 7.500000000000005329, -38.00000000000000000, 12.50000000000000000 ) ) ;
#8906 = CARTESIAN_POINT ( 'NONE',  ( -40.00000000000000711, 110.0000000000000000, -12.49999999999999645 ) ) ;
#8907 = ORIENTED_EDGE ( 'NONE', *, *, #15752, .F. ) ;
#8909 = EDGE_LOOP ( 'NONE', ( #12169, #10030, #15676, #13192, #1567, #3598 ) ) ;
#8908 = ORIENTED_EDGE ( 'NONE', *, *, #18567, .T. ) ;
#8910 = CARTESIAN_POINT ( 'NONE',  ( -9.020235676060220698, -27.64274437364852588, 21.76367750791695954 ) ) ;
#8911 = LINE ( 'NONE', #13314, #17747 ) ;
#8912 = EDGE_LOOP ( 'NONE', ( #487, #13091, #17146, #707 ) ) ;
#8913 = VECTOR ( 'NONE', #7288, 1000.000000000000000 ) ;
#8914 = ORIENTED_EDGE ( 'NONE', *, *, #17986, .T. ) ;
#8915 = CARTESIAN_POINT ( 'NONE',  ( -12.48433729119799196, -22.35725562635139596, 22.86132249208304401 ) ) ;
#8916 = CARTESIAN_POINT ( 'NONE',  ( 5.421010862427523748E-15, -25.00000000000000711, 0.000000000000000000 ) ) ;
#8917 = CARTESIAN_POINT ( 'NONE',  ( 32.50000000000000000, 47.00000000000000711, 12.50000000000000000 ) ) ;
#8918 = ORIENTED_EDGE ( 'NONE', *, *, #7122, .F. ) ;
#8919 = CARTESIAN_POINT ( 'NONE',  ( -18.04416526290808420, -24.63902057219074493, 7.982427507916962206 ) ) ;
#8920 = DIRECTION ( 'NONE',  ( 0.000000000000000000, 0.000000000000000000, 1.000000000000000000 ) ) ;
#8921 = ORIENTED_EDGE ( 'NONE', *, *, #2452, .F. ) ;
#8922 = EDGE_CURVE ( 'NONE', #16741, #7718, #17863, .T. ) ;
#8923 = CARTESIAN_POINT ( 'NONE',  ( 0.000000000000000000, -2.357898499370432610, 3.252606517456513302E-15 ) ) ;
#8924 = VERTEX_POINT ( 'NONE', #6493 ) ;
#8925 = DIRECTION ( 'NONE',  ( 0.7071067811865388020, -0.5000000000000074385, 0.5000000000000046629 ) ) ;
#8926 = LINE ( 'NONE', #1491, #15198 ) ;
#8927 = PRODUCT_DEFINITION_FORMATION_WITH_SPECIFIED_SOURCE ( 'ANY', '', #12163, .NOT_KNOWN. ) ;
#8928 = CARTESIAN_POINT ( 'NONE',  ( -24.00000000000000000, 53.00000000000000711, 30.00000000000000000 ) ) ;
#8929 = AXIS2_PLACEMENT_3D ( 'NONE', #11761, #113, #14714 ) ;
#8930 = APPLICATION_PROTOCOL_DEFINITION ( 'draft international standard', 'automotive_design', 1998, #14448 ) ;
#8931 = CARTESIAN_POINT ( 'NONE',  ( 1.767766952966370653, 62.23223304703363112, 46.40000000218494591 ) ) ;
#8932 = DIRECTION ( 'NONE',  ( 0.000000000000000000, -0.7071067811865495711, 0.7071067811865454633 ) ) ;
#8933 = CARTESIAN_POINT ( 'NONE',  ( -17.35725562635144215, -19.58745947852648683, 19.57617750791695954 ) ) ;
#8934 = CARTESIAN_POINT ( 'NONE',  ( 1.300000000000000044, 1.567547902908612085E-16, -1.280000000000000027 ) ) ;
#8935 = ORIENTED_EDGE ( 'NONE', *, *, #12424, .F. ) ;
#8936 = CARTESIAN_POINT ( 'NONE',  ( -15.16482700510263371, -18.99999999999997868, 0.9863224920830410136 ) ) ;
#8937 = VECTOR ( 'NONE', #6075, 1000.000000000000000 ) ;
#8938 = VECTOR ( 'NONE', #456, 1000.000000000000000 ) ;
#8939 = ADVANCED_FACE ( 'NONE', ( #8066 ), #15503, .F. ) ;
#8940 = CARTESIAN_POINT ( 'NONE',  ( -1.767766952966369765, 62.23223304703363112, 47.80000000218494449 ) ) ;
#8941 = CARTESIAN_POINT ( 'NONE',  ( -14.03132541760400009, -26.95583473709189448, 3.392572492083043567 ) ) ;
#8942 = CARTESIAN_POINT ( 'NONE',  ( 2.500000000000001776, 65.03553390593273775, 45.64999999999999858 ) ) ;
#8943 = EDGE_LOOP ( 'NONE', ( #16290, #1483, #858, #18898, #4193 ) ) ;
#8944 = DIRECTION ( 'NONE',  ( 0.000000000000000000, 0.000000000000000000, -1.000000000000000000 ) ) ;
#8945 = ORIENTED_EDGE ( 'NONE', *, *, #12920, .T. ) ;
#8946 = FACE_OUTER_BOUND ( 'NONE', #11431, .T. ) ;
#8947 = DIRECTION ( 'NONE',  ( 1.000000000000000000, -0.000000000000000000, -0.000000000000000000 ) ) ;
#8948 = DIRECTION ( 'NONE',  ( 0.000000000000000000, 1.000000000000000000, 0.000000000000000000 ) ) ;
#8949 = DIRECTION ( 'NONE',  ( 0.000000000000000000, -0.7071067811865492381, 0.7071067811865456854 ) ) ;
#8950 = CARTESIAN_POINT ( 'NONE',  ( 34.99999999999999289, 0.000000000000000000, 42.49999999999997868 ) ) ;
#8951 = ADVANCED_FACE ( 'NONE', ( #3828 ), #16882, .F. ) ;
#8952 = CARTESIAN_POINT ( 'NONE',  ( 3.796994071234847710E-16, 61.93301269999999903, 46.75000000109246656 ) ) ;
#8953 = CIRCLE ( 'NONE', #12699, 6.000000000000003553 ) ;
#8954 = AXIS2_PLACEMENT_3D ( 'NONE', #6031, #16811, #13861 ) ;
#8955 = PRODUCT ( 'socket head cap screw_iso_ISO 4762 M3 x 8 - 8N', 'socket head cap screw_iso_ISO 4762 M3 x 8 - 8N', '', ( #14620 ) ) ;
#8956 = PRESENTATION_STYLE_ASSIGNMENT (( #2975 ) ) ;
#8957 = CARTESIAN_POINT ( 'NONE',  ( -1.035533905932738863, 61.50000000000000000, 46.14999999999999858 ) ) ;
#8958 = LINE ( 'NONE', #14748, #12074 ) ;
#8959 = EDGE_LOOP ( 'NONE', ( #4826, #5662 ) ) ;
#8960 = FILL_AREA_STYLE_COLOUR ( '', #16764 ) ;
#8961 = CARTESIAN_POINT ( 'NONE',  ( -19.99999999999999645, -23.83517299489738051, 8.201177507916957765 ) ) ;
#8962 = CARTESIAN_POINT ( 'NONE',  ( -10.58745947852649927, -21.64274437364853654, 15.63867750791695777 ) ) ;
#8963 = CARTESIAN_POINT ( 'NONE',  ( -1.530808498934192803E-16, 66.50000000000000000, 45.00000000000000000 ) ) ;
#8964 = CARTESIAN_POINT ( 'NONE',  ( -20.00369391078757886, -29.24501739517668142, 41.01757249208304046 ) ) ;
#8965 = CIRCLE ( 'NONE', #10199, 2.999999999999999112 ) ;
#8966 = VECTOR ( 'NONE', #16987, 1000.000000000000000 ) ;
#8967 = CARTESIAN_POINT ( 'NONE',  ( -2.066987300000001415, 63.14382582708705627, 45.00000000109246656 ) ) ;
#8968 = CARTESIAN_POINT ( 'NONE',  ( -18.04416526290808420, -24.63902057219074493, 39.48242750791696665 ) ) ;
#8969 = LINE ( 'NONE', #14956, #12972 ) ;
#8970 = CARTESIAN_POINT ( 'NONE',  ( -9.999999999999994671, -24.16482700510257686, 5.576177507916958653 ) ) ;
#8971 = CARTESIAN_POINT ( 'NONE',  ( -41.00000000000000711, 113.0000000000000000, 30.00000000000000000 ) ) ;
#8972 = CARTESIAN_POINT ( 'NONE',  ( 1.461580736456473684, 65.46158073645646880, 49.45000000109246940 ) ) ;
#8973 = DIRECTION ( 'NONE',  ( 0.000000000000000000, -1.000000000000000000, 0.000000000000000000 ) ) ;
#8974 = DIRECTION ( 'NONE',  ( -0.000000000000000000, -0.000000000000000000, -1.000000000000000000 ) ) ;
#8975 = CARTESIAN_POINT ( 'NONE',  ( 2.066987300000001859, 63.14382582708704916, 45.30000000109246372 ) ) ;
#8976 = DIRECTION ( 'NONE',  ( -1.000000000000000000, 0.000000000000000000, 0.000000000000000000 ) ) ;
#8977 = CIRCLE ( 'NONE', #9295, 2.999999999999999112 ) ;
#8978 =( BOUNDED_CURVE ( )  B_SPLINE_CURVE ( 2, ( #16307, #1020, #10312, #11685, #16405, #10113, #7386, #8854, #13359 ),
 .UNSPECIFIED., .F., .F. ) 
 B_SPLINE_CURVE_WITH_KNOTS ( ( 3, 2, 2, 2, 3 ),
 ( 0.7142857142857141906, 0.7321428571428569843, 0.7500000000000000000, 0.7678571428571429047, 0.7857142857142856984 ),
 .UNSPECIFIED. ) 
 CURVE ( )  GEOMETRIC_REPRESENTATION_ITEM ( )  RATIONAL_B_SPLINE_CURVE ( ( 1.000000000000000444, 0.9238795325112862944, 1.000000000000000000, 0.9238795325112867385, 1.000000000000000000, 0.9238795325112867385, 1.000000000000000000, 0.9238795325112867385, 1.000000000000000000 ) ) 
 REPRESENTATION_ITEM ( '' )  );
#8979 = CARTESIAN_POINT ( 'NONE',  ( -3.065533689247737392, -45.28611686177728046, 3.000000000000000000 ) ) ;
#8980 = ORIENTED_EDGE ( 'NONE', *, *, #16453, .T. ) ;
#8981 = VERTEX_POINT ( 'NONE', #17077 ) ;
#8982 = CARTESIAN_POINT ( 'NONE',  ( -9.754982604823302594, -29.00369391078756465, 18.70507249208304046 ) ) ;
#8983 =( LENGTH_UNIT ( ) NAMED_UNIT ( * ) SI_UNIT ( .MILLI., .METRE. ) );
#8984 = DIRECTION ( 'NONE',  ( 1.000000000000000000, -0.000000000000000000, -0.000000000000000000 ) ) ;
#8986 = ORIENTED_EDGE ( 'NONE', *, *, #7145, .F. ) ;
#8985 = ORIENTED_EDGE ( 'NONE', *, *, #2913, .T. ) ;
#8987 = CARTESIAN_POINT ( 'NONE',  ( -14.83517299489738761, -20.99999999999997513, 9.513677507916957765 ) ) ;
#8988 = CARTESIAN_POINT ( 'NONE',  ( -2.500000000000001776, 64.00000000000000000, 48.50000000218494023 ) ) ;
#8989 = CARTESIAN_POINT ( 'NONE',  ( -21.99999999999999289, -23.83517299489739116, 39.70117750791695954 ) ) ;
#8990 = CARTESIAN_POINT ( 'NONE',  ( -0.8561741729129461742, 66.06698729999999387, 49.40000000109247225 ) ) ;
#8991 = CARTESIAN_POINT ( 'NONE',  ( -2.066987300000001415, 64.00000000000000000, 49.55000000109247082 ) ) ;
#8992 = ORIENTED_EDGE ( 'NONE', *, *, #2352, .T. ) ;
#8993 = ORIENTED_EDGE ( 'NONE', *, *, #13088, .F. ) ;
#8994 = EDGE_CURVE ( 'NONE', #9118, #14005, #2166, .T. ) ;
#8995 = EDGE_CURVE ( 'NONE', #8015, #16369, #14220, .T. ) ;
#8996 = LINE ( 'NONE', #19101, #17889 ) ;
#8997 = PLANE ( 'NONE',  #398 ) ;
#8998 = ORIENTED_EDGE ( 'NONE', *, *, #13265, .F. ) ;
#8999 = CARTESIAN_POINT ( 'NONE',  ( 1.300000000000000044, -0.7390083445627200209, 1.280000000000001137 ) ) ;
#9000 = CARTESIAN_POINT ( 'NONE',  ( 4.012830983233651061, 32.52836399182262994, 53.60336399182268252 ) ) ;
#9001 = EDGE_CURVE ( 'NONE', #12626, #16767, #11272, .T. ) ;
#9002 = CARTESIAN_POINT ( 'NONE',  ( -0.8561741729129465073, 61.93301270000000613, 47.50000000109246656 ) ) ;
#9003 = DIRECTION ( 'NONE',  ( -1.000000000000000000, -0.000000000000000000, -0.000000000000000000 ) ) ;
#9004 = ADVANCED_FACE ( 'NONE', ( #4931 ), #2827, .T. ) ;
#9005 = FACE_OUTER_BOUND ( 'NONE', #8019, .T. ) ;
#9006 = ORIENTED_EDGE ( 'NONE', *, *, #124, .T. ) ;
#9008 = VERTEX_POINT ( 'NONE', #1982 ) ;
#9007 = EDGE_LOOP ( 'NONE', ( #2045, #4816, #19020, #17409 ) ) ;
#9009 = CARTESIAN_POINT ( 'NONE',  ( -21.95583473709191580, -21.95952864787954084, 13.66992750791695954 ) ) ;
#9010 = DIRECTION ( 'NONE',  ( -0.9863224920830415687, -6.131453374264637327E-15, -0.1648270051026182181 ) ) ;
#9011 = ORIENTED_EDGE ( 'NONE', *, *, #15306, .T. ) ;
#9012 = ORIENTED_EDGE ( 'NONE', *, *, #1210, .T. ) ;
#9013 = CARTESIAN_POINT ( 'NONE',  ( -12.48433729119799196, -22.35725562635139596, 17.61132249208304401 ) ) ;
#9014 = EDGE_CURVE ( 'NONE', #3722, #13544, #6684, .T. ) ;
#9015 = CARTESIAN_POINT ( 'NONE',  ( 37.50000000000000711, 0.000000000000000000, -45.00000000000000000 ) ) ;
#9016 = DIRECTION ( 'NONE',  ( 0.000000000000000000, 0.000000000000000000, 1.000000000000000000 ) ) ;
#9017 = VERTEX_POINT ( 'NONE', #17261 ) ;
#9018 = CARTESIAN_POINT ( 'NONE',  ( -11.99999999999999289, -24.16482700510258752, 10.82617750791695954 ) ) ;
#9019 = CARTESIAN_POINT ( 'NONE',  ( -24.00000000000000000, 52.00000000000000711, -67.72004514666936359 ) ) ;
#9020 = ORIENTED_EDGE ( 'NONE', *, *, #13706, .T. ) ;
#9021 = DIRECTION ( 'NONE',  ( 3.491481338843133355E-15, 0.7071067811865495711, -0.7071067811865454633 ) ) ;
#9022 = ORIENTED_EDGE ( 'NONE', *, *, #11659, .F. ) ;
#9023 = EDGE_CURVE ( 'NONE', #7944, #7050, #17168, .T. ) ;
#9024 = DIRECTION ( 'NONE',  ( 0.000000000000000000, 0.000000000000000000, 1.000000000000000000 ) ) ;
#9025 = FACE_OUTER_BOUND ( 'NONE', #13534, .T. ) ;
#9026 = DIRECTION ( 'NONE',  ( -1.000000000000000000, 0.000000000000000000, -0.000000000000000000 ) ) ;
#9027 = APPLICATION_PROTOCOL_DEFINITION ( 'draft international standard', 'automotive_design', 1998, #18841 ) ;
#9028 = LINE ( 'NONE', #13539, #16986 ) ;
#9029 = AXIS2_PLACEMENT_3D ( 'NONE', #18985, #12896, #5457 ) ;
#9030 = CARTESIAN_POINT ( 'NONE',  ( -19.99999999999999645, -23.83517299489738051, 34.45117750791696665 ) ) ;
#9031 = FACE_OUTER_BOUND ( 'NONE', #11346, .T. ) ;
#9032 = CARTESIAN_POINT ( 'NONE',  ( -19.41254052147348830, -26.35725562635142083, 23.51367750791695954 ) ) ;
#9033 = CARTESIAN_POINT ( 'NONE',  ( -17.70357423236093553, -43.78611686177728046, 3.000000000000000000 ) ) ;
#9034 = ADVANCED_FACE ( 'NONE', ( #10888 ), #18648, .F. ) ;
#9035 = ORIENTED_EDGE ( 'NONE', *, *, #10033, .F. ) ;
#9036 = EDGE_CURVE ( 'NONE', #17270, #18191, #7966, .T. ) ;
#9037 = UNCERTAINTY_MEASURE_WITH_UNIT (LENGTH_MEASURE( 1.000000000000000082E-05 ), #653, 'distance_accuracy_value', 'NONE');
#9038 = CARTESIAN_POINT ( 'NONE',  ( -12.35725562635140307, -28.24771351637085459, 24.17382249208304046 ) ) ;
#9039 = VECTOR ( 'NONE', #11165, 1000.000000000000000 ) ;
#9040 = CARTESIAN_POINT ( 'NONE',  ( 0.8561741729129460632, 66.06698729999999387, 45.30000000109247082 ) ) ;
#9041 = EDGE_CURVE ( 'NONE', #4229, #2520, #12361, .T. ) ;
#9042 = CARTESIAN_POINT ( 'NONE',  ( -12.48433729119799196, -22.35725562635139596, 1.861322492083043123 ) ) ;
#9043 = CIRCLE ( 'NONE', #19062, 1.000000000000000000 ) ;
#9044 = CARTESIAN_POINT ( 'NONE',  ( -41.00000000000000711, 110.0000000000000000, 13.50000000000000000 ) ) ;
#9045 = ORIENTED_EDGE ( 'NONE', *, *, #17392, .F. ) ;
#9046 = CARTESIAN_POINT ( 'NONE',  ( -14.69695850531174131, -17.99999999999998934, -4.336808689941901379E-16 ) ) ;
#9047 = ORIENTED_EDGE ( 'NONE', *, *, #13917, .T. ) ;
#9048 = CYLINDRICAL_SURFACE ( 'NONE', #6868, 2.500000000000001776 ) ;
#9049 = DIRECTION ( 'NONE',  ( -0.000000000000000000, -1.000000000000000000, -0.000000000000000000 ) ) ;
#9050 = FACE_BOUND ( 'NONE', #19086, .T. ) ;
#9051 = CYLINDRICAL_SURFACE ( 'NONE', #345, 2.500000000000001776 ) ;
#9052 = CARTESIAN_POINT ( 'NONE',  ( 2.066987300000001415, 64.00000000000000000, 45.35000000109246798 ) ) ;
#9053 = EDGE_CURVE ( 'NONE', #9118, #7333, #13838, .T. ) ;
#9054 = CARTESIAN_POINT ( 'NONE',  ( 11.83926609531033058, -43.78611686177728046, 3.000000000000000000 ) ) ;
#9055 = CARTESIAN_POINT ( 'NONE',  ( 1.767766952966369987, 65.76776695296638309, 47.29999999999999716 ) ) ;
#9056 = CARTESIAN_POINT ( 'NONE',  ( -24.00000000000000000, 113.0000000000000000, -50.00000000000000000 ) ) ;
#9057 = VECTOR ( 'NONE', #9147, 1000.000000000000000 ) ;
#9058 = AXIS2_PLACEMENT_3D ( 'NONE', #7936, #754, #567 ) ;
#9059 = ORIENTED_EDGE ( 'NONE', *, *, #2404, .F. ) ;
#9060 = CARTESIAN_POINT ( 'NONE',  ( 0.000000000000000000, 0.000000000000000000, 0.000000000000000000 ) ) ;
#9061 = CARTESIAN_POINT ( 'NONE',  ( -19.24771351637089367, -21.35725562635142438, 19.13867750791695954 ) ) ;
#9062 = CARTESIAN_POINT ( 'NONE',  ( -11.21908421996108629, -20.46040770435011069, 10.16992750791695244 ) ) ;
#9063 = CARTESIAN_POINT ( 'NONE',  ( 4.592425496802577917E-16, 61.50000000000000000, 47.90000000218494591 ) ) ;
#9064 = CARTESIAN_POINT ( 'NONE',  ( -22.04416526290809486, -22.28918265808477628, 41.89257249208304046 ) ) ;
#9065 = VECTOR ( 'NONE', #11900, 1000.000000000000000 ) ;
#9066 = LINE ( 'NONE', #1631, #2266 ) ;
#9067 = CARTESIAN_POINT ( 'NONE',  ( -13.49542703274178379, -19.04416526290806289, -0.7675724920830416798 ) ) ;
#9068 =( REPRESENTATION_RELATIONSHIP ('NONE','NONE', #7912, #8522 ) REPRESENTATION_RELATIONSHIP_WITH_TRANSFORMATION ( #12557 )SHAPE_REPRESENTATION_RELATIONSHIP( ) );
#9069 = CARTESIAN_POINT ( 'NONE',  ( 10.71950000000001424, 0.000000000000000000, 0.000000000000000000 ) ) ;
#9070 = CARTESIAN_POINT ( 'NONE',  ( -10.04416526290807710, -25.50457296725819489, 21.54492750791695599 ) ) ;
#9071 = AXIS2_PLACEMENT_3D ( 'NONE', #11163, #11441, #17160 ) ;
#9072 = LINE ( 'NONE', #62, #15921 ) ;
#9073 = DIRECTION ( 'NONE',  ( -0.000000000000000000, -1.000000000000000000, -0.000000000000000000 ) ) ;
#9074 = DIRECTION ( 'NONE',  ( 0.000000000000000000, 0.000000000000000000, 1.000000000000000000 ) ) ;
#9075 = PLANE ( 'NONE',  #11609 ) ;
#9076 = AXIS2_PLACEMENT_3D ( 'NONE', #8240, #16868, #1868 ) ;
#9077 = EDGE_CURVE ( 'NONE', #9, #16792, #12457, .T. ) ;
#9078 = CARTESIAN_POINT ( 'NONE',  ( -1.461580736456473906, 65.46158073645646880, 46.45000000109246940 ) ) ;
#9079 = CARTESIAN_POINT ( 'NONE',  ( -2.066987300000001415, 64.00000000000000000, 49.75000000109246656 ) ) ;
#9080 = CARTESIAN_POINT ( 'NONE',  ( -0.08838834764832756430, 29.68014068711926257, 56.80514068711929809 ) ) ;
#9081 = AXIS2_PLACEMENT_3D ( 'NONE', #1977, #6294, #3724 ) ;
#9082 = FACE_OUTER_BOUND ( 'NONE', #14363, .T. ) ;
#9083 = ORIENTED_EDGE ( 'NONE', *, *, #18834, .F. ) ;
#9084 = ORIENTED_EDGE ( 'NONE', *, *, #16958, .F. ) ;
#9085 = CARTESIAN_POINT ( 'NONE',  ( -18.64274437364860049, -18.02023567606023491, 16.29882249208303691 ) ) ;
#9086 = CARTESIAN_POINT ( 'NONE',  ( -11.21908421996106142, -27.53959229564982181, 2.955072492083040903 ) ) ;
#9088 = VERTEX_POINT ( 'NONE', #18360 ) ;
#9087 = ORIENTED_EDGE ( 'NONE', *, *, #11983, .T. ) ;
#9089 = CARTESIAN_POINT ( 'NONE',  ( -17.51566270880201159, -22.35725562635141728, 8.638677507916959541 ) ) ;
#9090 = DIRECTION ( 'NONE',  ( 0.000000000000000000, 0.000000000000000000, -1.000000000000000000 ) ) ;
#9091 = CARTESIAN_POINT ( 'NONE',  ( -9.996306089212408708, -18.75498260482328661, 6.892572492083038682 ) ) ;
#9092 = VECTOR ( 'NONE', #2767, 999.9999999999998863 ) ;
#9093 = CARTESIAN_POINT ( 'NONE',  ( -0.8561741729129465073, 61.93301270000000613, 48.10000000109246798 ) ) ;
#9094 = CARTESIAN_POINT ( 'NONE',  ( -1.265664690411616068E-16, 66.06698730000000808, 46.95000000109246940 ) ) ;
#9095 = VERTEX_POINT ( 'NONE', #18559 ) ;
#9096 = ORIENTED_EDGE ( 'NONE', *, *, #10373, .T. ) ;
#9097 = CARTESIAN_POINT ( 'NONE',  ( -2.500000000000001776, 64.00000000000000000, 46.10000000218494165 ) ) ;
#9098 = VERTEX_POINT ( 'NONE', #10984 ) ;
#9099 = VECTOR ( 'NONE', #9127, 1000.000000000000000 ) ;
#9100 = VERTEX_POINT ( 'NONE', #3729 ) ;
#9101 = CARTESIAN_POINT ( 'NONE',  ( -12.64915539091913566, -20.59698958850244210, -1.847635612036354826E-16 ) ) ;
#9102 = CARTESIAN_POINT ( 'NONE',  ( 2.500000000000001776, 64.00000000000000000, 46.50000000218494733 ) ) ;
#9103 = CARTESIAN_POINT ( 'NONE',  ( -2.066987300000001859, 64.85617417291294373, 48.90000000109247225 ) ) ;
#9104 = LINE ( 'NONE', #282, #11904 ) ;
#9105 = LINE ( 'NONE', #16759, #6770 ) ;
#9106 = VERTEX_POINT ( 'NONE', #5127 ) ;
#9108 = ORIENTED_EDGE ( 'NONE', *, *, #7466, .T. ) ;
#9107 = ORIENTED_EDGE ( 'NONE', *, *, #4989, .F. ) ;
#9109 = CARTESIAN_POINT ( 'NONE',  ( -17.04047135212043784, -30.95583473709190159, 12.35742750791695777 ) ) ;
#9110 = CARTESIAN_POINT ( 'NONE',  ( -1.035533905932738641, 66.50000000000000000, 45.04999999999999005 ) ) ;
#9111 = VECTOR ( 'NONE', #11375, 1000.000000000000000 ) ;
#9112 = ORIENTED_EDGE ( 'NONE', *, *, #19242, .F. ) ;
#9113 = ORIENTED_EDGE ( 'NONE', *, *, #18416, .F. ) ;
#9114 = CARTESIAN_POINT ( 'NONE',  ( -12.68318583509882380, -26.07549068051207541, 18.70507249208304401 ) ) ;
#9115 = VECTOR ( 'NONE', #12899, 1000.000000000000000 ) ;
#9116 = CARTESIAN_POINT ( 'NONE',  ( -2.066987300000001415, 64.00000000000000000, 47.95000000109246940 ) ) ;
#9117 = LINE ( 'NONE', #3139, #9383 ) ;
#9118 = VERTEX_POINT ( 'NONE', #11080 ) ;
#9119 = CARTESIAN_POINT ( 'NONE',  ( -18.04416526290808420, -24.63902057219074493, 13.23242750791696132 ) ) ;
#9120 = ADVANCED_FACE ( 'NONE', ( #702 ), #18510, .F. ) ;
#9121 = VECTOR ( 'NONE', #15937, 1000.000000000000000 ) ;
#9122 = CARTESIAN_POINT ( 'NONE',  ( -50.00000000000002132, 33.00000000000000000, 40.49999999999996447 ) ) ;
#9123 = ORIENTED_EDGE ( 'NONE', *, *, #9299, .T. ) ;
#9124 = LINE ( 'NONE', #5894, #6603 ) ;
#9125 = PRODUCT_DEFINITION_SHAPE ( 'NONE', 'NONE',  #11688 ) ;
#9126 = ORIENTED_EDGE ( 'NONE', *, *, #18946, .T. ) ;
#9127 = DIRECTION ( 'NONE',  ( 1.000000000000000000, -0.000000000000000000, 0.000000000000000000 ) ) ;
#9128 = LINE ( 'NONE', #16281, #3919 ) ;
#9129 = LINE ( 'NONE', #8928, #9733 ) ;
#9130 = AXIS2_PLACEMENT_3D ( 'NONE', #9673, #18795, #5650 ) ;
#9131 = ITEM_DEFINED_TRANSFORMATION ( 'NONE', 'NONE', #158,  #1791 ) ;
#9132 = DIRECTION ( 'NONE',  ( -0.000000000000000000, -1.000000000000000000, 0.000000000000000000 ) ) ;
#9133 = CARTESIAN_POINT ( 'NONE',  ( -25.00000000000000711, 53.00000000000000711, -44.00000000000000000 ) ) ;
#9134 = CIRCLE ( 'NONE', #5691, 2.500000000000002220 ) ;
#9135 = CARTESIAN_POINT ( 'NONE',  ( -4.101219330882018177, 26.84264068711928530, 59.64264068711926825 ) ) ;
#9136 = FACE_OUTER_BOUND ( 'NONE', #19186, .T. ) ;
#9137 = EDGE_CURVE ( 'NONE', #2714, #9379, #15696, .T. ) ;
#9138 = CARTESIAN_POINT ( 'NONE',  ( -13.82508104294698192, -29.04416526290806644, 17.16992750791694888 ) ) ;
#9139 = CARTESIAN_POINT ( 'NONE',  ( -40.00000000000000711, 110.0000000000000000, -37.50000000000000711 ) ) ;
#9140 = VERTEX_POINT ( 'NONE', #6774 ) ;
#9141 = CARTESIAN_POINT ( 'NONE',  ( -14.83517299489735741, -28.99999999999998224, 14.11132249208304046 ) ) ;
#9142 = FACE_BOUND ( 'NONE', #13322, .T. ) ;
#9143 = CARTESIAN_POINT ( 'NONE',  ( -17.31681416490117087, -21.92450931948788551, 16.08007249208304401 ) ) ;
#9144 = CIRCLE ( 'NONE', #10378, 1.500000000000001332 ) ;
#9145 = CARTESIAN_POINT ( 'NONE',  ( 2.500000000000001776, 64.00000000000000000, 45.59999999999999432 ) ) ;
#9146 = ORIENTED_EDGE ( 'NONE', *, *, #7714, .F. ) ;
#9147 = DIRECTION ( 'NONE',  ( 1.000000000000000000, -0.000000000000000000, -0.000000000000000000 ) ) ;
#9148 = ORIENTED_EDGE ( 'NONE', *, *, #9455, .T. ) ;
#9149 = FACE_OUTER_BOUND ( 'NONE', #12753, .T. ) ;
#9150 = LINE ( 'NONE', #1802, #2639 ) ;
#9151 = DIRECTION ( 'NONE',  ( 0.000000000000000000, 0.000000000000000000, 1.000000000000000000 ) ) ;
#9152 = EDGE_CURVE ( 'NONE', #7260, #4550, #7045, .T. ) ;
#9153 = ADVANCED_FACE ( 'NONE', ( #9887 ), #19207, .T. ) ;
#9154 = CARTESIAN_POINT ( 'NONE',  ( -0.8561741729129466183, 61.93301270000000613, 46.70000000109248361 ) ) ;
#9155 = ADVANCED_FACE ( 'NONE', ( #8338 ), #17537, .T. ) ;
#9156 = DIRECTION ( 'NONE',  ( 0.000000000000000000, -1.000000000000000000, 0.000000000000000000 ) ) ;
#9157 = LINE ( 'NONE', #6421, #1613 ) ;
#9158 = LINE ( 'NONE', #15332, #3638 ) ;
#9159 = VERTEX_POINT ( 'NONE', #4012 ) ;
#9160 = CARTESIAN_POINT ( 'NONE',  ( 44.99999999999997158, -3.000000000000002665, 55.00000000000000000 ) ) ;
#9161 = CARTESIAN_POINT ( 'NONE',  ( -11.21908421996108629, -20.46040770435011069, 15.41992750791695954 ) ) ;
#9162 = CARTESIAN_POINT ( 'NONE',  ( -9.955834737091912245, -22.82508104294696594, 10.60742750791695777 ) ) ;
#9163 = CARTESIAN_POINT ( 'NONE',  ( -2.500000000000001776, 64.00000000000000000, 49.30000000218494449 ) ) ;
#9164 = CARTESIAN_POINT ( 'NONE',  ( -10.75228648362912232, -21.35725562635138530, 22.86132249208304401 ) ) ;
#9165 = CARTESIAN_POINT ( 'NONE',  ( 0.8561741729129472844, 61.93301270000000613, 46.00000000109245946 ) ) ;
#9166 = EDGE_CURVE ( 'NONE', #6401, #9696, #17348, .T. ) ;
#9167 = CARTESIAN_POINT ( 'NONE',  ( -15.96867458239597326, -26.95583473709190159, 38.60742750791696665 ) ) ;
#9168 = ADVANCED_FACE ( 'NONE', ( #2627 ), #5683, .T. ) ;
#9169 = DIRECTION ( 'NONE',  ( -0.7071067811865561215, -0.4999999999999953926, 0.4999999999999925060 ) ) ;
#9170 = CARTESIAN_POINT ( 'NONE',  ( -17.35725562635144215, -19.58745947852648683, 14.32617750791695777 ) ) ;
#9171 = LINE ( 'NONE', #18098, #8196 ) ;
#9172 = DIRECTION ( 'NONE',  ( 1.000000000000000000, 0.000000000000000000, 2.973811673103096679E-16 ) ) ;
#9173 = CARTESIAN_POINT ( 'NONE',  ( -1.461580736456473462, 62.53841926354353120, 46.65000000109247225 ) ) ;
#9174 = CARTESIAN_POINT ( 'NONE',  ( 2.750000000000009326, 37.99999999999999289, 37.49999999999996447 ) ) ;
#9175 = FACE_OUTER_BOUND ( 'NONE', #1256, .T. ) ;
#9176 = CARTESIAN_POINT ( 'NONE',  ( -41.00000000000000711, 53.00000000000000711, 21.00000000000000000 ) ) ;
#9177 = DIRECTION ( 'NONE',  ( 0.000000000000000000, 1.000000000000000000, -0.000000000000000000 ) ) ;
#9178 = CARTESIAN_POINT ( 'NONE',  ( -41.00000000000000711, 53.00000000000000711, -6.000000000000001776 ) ) ;
#9179 = CARTESIAN_POINT ( 'NONE',  ( 11.83926609531033058, -43.78611686177728046, 1.500000000000000000 ) ) ;
#9180 = ORIENTED_EDGE ( 'NONE', *, *, #17190, .F. ) ;
#9181 = ORIENTED_EDGE ( 'NONE', *, *, #5923, .T. ) ;
#9182 = PRODUCT_DEFINITION ( 'UNKNOWN', '', #9237, #11576 ) ;
#9183 = CARTESIAN_POINT ( 'NONE',  ( -9.996306089212408708, -18.75498260482328661, 17.39257249208304046 ) ) ;
#9184 = CARTESIAN_POINT ( 'NONE',  ( -12.35725562635140307, -28.24771351637085459, 8.423822492083042235 ) ) ;
#9186 = ORIENTED_EDGE ( 'NONE', *, *, #5234, .F. ) ;
#9185 = VERTEX_POINT ( 'NONE', #1268 ) ;
#9187 = CARTESIAN_POINT ( 'NONE',  ( -14.03132541760401786, -21.04416526290806289, 20.23242750791696309 ) ) ;
#9188 = CARTESIAN_POINT ( 'NONE',  ( -2.499999999999999556, 62.96446609406726225, 48.55000000218494449 ) ) ;
#9189 = CARTESIAN_POINT ( 'NONE',  ( -20.24501739517669563, -18.99630608921239627, 10.83007249208304046 ) ) ;
#9190 = CARTESIAN_POINT ( 'NONE',  ( -2.066987300000001415, 64.00000000000000000, 48.75000000109246656 ) ) ;
#9191 = CARTESIAN_POINT ( 'NONE',  ( 0.8561741729129460632, 66.06698729999999387, 46.90000000109247225 ) ) ;
#9192 = ORIENTED_EDGE ( 'NONE', *, *, #7767, .T. ) ;
#9193 = ADVANCED_FACE ( 'NONE', ( #8521 ), #14311, .T. ) ;
#9194 = ORIENTED_EDGE ( 'NONE', *, *, #14818, .F. ) ;
#9195 = DIRECTION ( 'NONE',  ( -1.000000000000000000, -0.000000000000000000, -0.000000000000000000 ) ) ;
#9196 = CARTESIAN_POINT ( 'NONE',  ( -32.50000000000000000, 52.00000000000000711, 12.34999999999999964 ) ) ;
#9197 = EDGE_LOOP ( 'NONE', ( #10815, #2459, #368, #12906, #6077, #3107, #10572, #14233 ) ) ;
#9198 = DIRECTION ( 'NONE',  ( 0.8660254037844385966, 0.000000000000000000, 0.5000000000000001110 ) ) ;
#9199 = LINE ( 'NONE', #18127, #14073 ) ;
#9200 = DIRECTION ( 'NONE',  ( -1.000000000000000000, 0.000000000000000000, 0.000000000000000000 ) ) ;
#9201 = CARTESIAN_POINT ( 'NONE',  ( 32.50000000000000000, 52.00000000000000711, 12.50000000000000000 ) ) ;
#9202 = LINE ( 'NONE', #6180, #12992 ) ;
#9203 = ORIENTED_EDGE ( 'NONE', *, *, #2246, .T. ) ;
#9205 = ORIENTED_EDGE ( 'NONE', *, *, #3519, .T. ) ;
#9204 = VERTEX_POINT ( 'NONE', #2733 ) ;
#9206 = CARTESIAN_POINT ( 'NONE',  ( -21.14459132904236327, -27.35725562635143149, 18.26367750791695599 ) ) ;
#9207 = ORIENTED_EDGE ( 'NONE', *, *, #11832, .F. ) ;
#9208 = VERTEX_POINT ( 'NONE', #19111 ) ;
#9209 = CARTESIAN_POINT ( 'NONE',  ( -12.92450931948790149, -21.68318583509881137, 12.14257249208304223 ) ) ;
#9210 = CARTESIAN_POINT ( 'NONE',  ( -19.24771351637089367, -21.35725562635142438, 40.13867750791695954 ) ) ;
#9211 = VECTOR ( 'NONE', #3278, 1000.000000000000000 ) ;
#9212 = CARTESIAN_POINT ( 'NONE',  ( 2.066987300000001415, 64.85617417291294373, 47.60000000109246798 ) ) ;
#9213 = DIRECTION ( 'NONE',  ( 0.000000000000000000, -0.7071067811865493491, 0.7071067811865456854 ) ) ;
#9214 = ORIENTED_EDGE ( 'NONE', *, *, #15716, .F. ) ;
#9215 = CARTESIAN_POINT ( 'NONE',  ( -12.48433729119798130, -25.64274437364855075, 21.76367750791695954 ) ) ;
#9216 = CARTESIAN_POINT ( 'NONE',  ( -40.00000000000000711, 113.0000000000000000, 14.50000000000000000 ) ) ;
#9217 = ORIENTED_EDGE ( 'NONE', *, *, #6013, .T. ) ;
#9218 = CARTESIAN_POINT ( 'NONE',  ( -24.00000000000000000, 53.00000000000000711, -25.49999999999999645 ) ) ;
#9219 = ORIENTED_EDGE ( 'NONE', *, *, #7218, .T. ) ;
#9220 = SURFACE_SIDE_STYLE ('',( #1875 ) ) ;
#9221 = CARTESIAN_POINT ( 'NONE',  ( -2.500000000000001776, 64.00000000000000000, 49.99999999999999289 ) ) ;
#9222 = DIRECTION ( 'NONE',  ( 0.000000000000000000, 0.000000000000000000, -1.000000000000000000 ) ) ;
#9223 = CARTESIAN_POINT ( 'NONE',  ( -40.00000000000000711, 110.0000000000000000, -44.00000000000000000 ) ) ;
#9224 = PLANE ( 'NONE',  #17417 ) ;
#9225 = DIRECTION ( 'NONE',  ( -0.000000000000000000, -0.7071067811865456854, -0.7071067811865493491 ) ) ;
#9226 =( GEOMETRIC_REPRESENTATION_CONTEXT ( 3 ) GLOBAL_UNCERTAINTY_ASSIGNED_CONTEXT ( ( #4939 ) ) GLOBAL_UNIT_ASSIGNED_CONTEXT ( ( #17400, #14179, #5543 ) ) REPRESENTATION_CONTEXT ( 'NONE', 'WORKASPACE' ) );
#9227 = CARTESIAN_POINT ( 'NONE',  ( -13.82508104294698192, -29.04416526290806644, 38.16992750791695244 ) ) ;
#9228 = VECTOR ( 'NONE', #9645, 1000.000000000000000 ) ;
#9229 = PLANE ( 'NONE',  #9863 ) ;
#9230 = ORIENTED_EDGE ( 'NONE', *, *, #7832, .F. ) ;
#9231 = CARTESIAN_POINT ( 'NONE',  ( -10.58745947852649927, -21.64274437364853654, 10.38867750791695777 ) ) ;
#9232 = CARTESIAN_POINT ( 'NONE',  ( -25.00000000000000000, 53.00000000000000711, 27.50000000000000000 ) ) ;
#9233 = EDGE_LOOP ( 'NONE', ( #13092, #4088, #9721, #12536 ) ) ;
#9234 = CARTESIAN_POINT ( 'NONE',  ( -12.64274437364858628, -19.58745947852646552, 11.92382249208304223 ) ) ;
#9235 = DIRECTION ( 'NONE',  ( -0.000000000000000000, -0.000000000000000000, -1.000000000000000000 ) ) ;
#9236 = CARTESIAN_POINT ( 'NONE',  ( -12.68318583509882380, -26.07549068051207541, 18.70507249208304401 ) ) ;
#9237 = PRODUCT_DEFINITION_FORMATION_WITH_SPECIFIED_SOURCE ( 'ANY', '', #12997, .NOT_KNOWN. ) ;
#9238 = PLANE ( 'NONE',  #342 ) ;
#9239 = VERTEX_POINT ( 'NONE', #978 ) ;
#9240 = AXIS2_PLACEMENT_3D ( 'NONE', #15325, #9628, #18669 ) ;
#9241 = FACE_OUTER_BOUND ( 'NONE', #49, .T. ) ;
#9242 = ORIENTED_EDGE ( 'NONE', *, *, #10546, .F. ) ;
#9243 = FACE_OUTER_BOUND ( 'NONE', #16761, .T. ) ;
#9244 = EDGE_CURVE ( 'NONE', #9, #1049, #18185, .T. ) ;
#9245 = EDGE_CURVE ( 'NONE', #11147, #15003, #10331, .T. ) ;
#9246 = DIRECTION ( 'NONE',  ( -0.000000000000000000, -0.000000000000000000, 1.000000000000000000 ) ) ;
#9247 = LINE ( 'NONE', #1804, #4083 ) ;
#9248 = CARTESIAN_POINT ( 'NONE',  ( 44.99999999999998579, 6.000000000000000000, -53.49999999999998579 ) ) ;
#9249 = DIRECTION ( 'NONE',  ( 0.000000000000000000, -1.000000000000000000, 0.000000000000000000 ) ) ;
#9250 = CARTESIAN_POINT ( 'NONE',  ( -25.00000000000000000, 110.0000000000000000, 30.00000000000000000 ) ) ;
#9251 = VECTOR ( 'NONE', #9706, 1000.000000000000114 ) ;
#9252 = VECTOR ( 'NONE', #14783, 1000.000000000000000 ) ;
#9253 = ORIENTED_EDGE ( 'NONE', *, *, #11422, .F. ) ;
#9254 = DIRECTION ( 'NONE',  ( 0.000000000000000000, 1.000000000000000000, 0.000000000000000000 ) ) ;
#9255 = CARTESIAN_POINT ( 'NONE',  ( -10.04416526290807710, -25.50457296725819489, 11.04492750791695421 ) ) ;
#9256 = EDGE_CURVE ( 'NONE', #2227, #13385, #16067, .T. ) ;
#9257 = CARTESIAN_POINT ( 'NONE',  ( 1.767766952966369987, 65.76776695296638309, 45.00000000218494733 ) ) ;
#9258 = ADVANCED_FACE ( 'NONE', ( #8425 ), #14598, .F. ) ;
#9259 = CARTESIAN_POINT ( 'NONE',  ( -13.82508104294702100, -18.95583473709188382, 16.95507249208304046 ) ) ;
#9260 = CARTESIAN_POINT ( 'NONE',  ( 2.066987300000001415, 64.00000000000000000, 45.35000000109246798 ) ) ;
#9261 = CARTESIAN_POINT ( 'NONE',  ( -10.75228648362910100, -26.64274437364854009, 21.76367750791695599 ) ) ;
#9262 = CARTESIAN_POINT ( 'NONE',  ( -41.00000000000000711, 53.00000000000000711, 6.999999999999999112 ) ) ;
#9263 = AXIS2_PLACEMENT_3D ( 'NONE', #14284, #17049, #9947 ) ;
#9264 = CARTESIAN_POINT ( 'NONE',  ( -19.99999999999999645, -23.83517299489738051, 13.45117750791695777 ) ) ;
#9265 = LINE ( 'NONE', #12202, #11222 ) ;
#9266 = CARTESIAN_POINT ( 'NONE',  ( -0.1250000000000104083, 33.66708332270461312, 52.46464466094069934 ) ) ;
#9267 = VECTOR ( 'NONE', #11991, 1000.000000000000000 ) ;
#9268 = CARTESIAN_POINT ( 'NONE',  ( -2.066987300000001415, 64.00000000000000000, 48.95000000109246940 ) ) ;
#9269 = CARTESIAN_POINT ( 'NONE',  ( -25.00000000000000000, 53.00000000000000711, 0.5000000000000004441 ) ) ;
#9270 = DIRECTION ( 'NONE',  ( 0.7071067811865437980, -0.5000000000000044409, 0.5000000000000008882 ) ) ;
#9271 = CARTESIAN_POINT ( 'NONE',  ( 2.500000000000001776, 64.00000000000000000, 48.10000000218494165 ) ) ;
#9272 = CARTESIAN_POINT ( 'NONE',  ( -2.066987300000001415, 63.14382582708705627, 48.20000000109247651 ) ) ;
#9273 = DIRECTION ( 'NONE',  ( 1.000000000000000000, -0.000000000000000000, 0.000000000000000000 ) ) ;
#9274 = VERTEX_POINT ( 'NONE', #17634 ) ;
#9275 = VERTEX_POINT ( 'NONE', #1068 ) ;
#9276 = CARTESIAN_POINT ( 'NONE',  ( -22.04416526290809486, -22.28918265808477628, 36.64257249208304046 ) ) ;
#9277 = VECTOR ( 'NONE', #15886, 1000.000000000000000 ) ;
#9278 = EDGE_CURVE ( 'NONE', #17318, #9490, #6855, .T. ) ;
#9279 = CARTESIAN_POINT ( 'NONE',  ( -19.41254052147350961, -21.64274437364857562, 10.61132249208304046 ) ) ;
#9281 = EDGE_LOOP ( 'NONE', ( #3162, #6183, #12726, #18845 ) ) ;
#9280 = EDGE_CURVE ( 'NONE', #4229, #10346, #1165, .T. ) ;
#9282 = CARTESIAN_POINT ( 'NONE',  ( -15.16482700510260706, -26.99999999999998579, 12.13867750791695954 ) ) ;
#9283 = LINE ( 'NONE', #14085, #802 ) ;
#9284 = CARTESIAN_POINT ( 'NONE',  ( -13.28918265808478694, -16.95583473709189093, 22.20507249208304046 ) ) ;
#9285 = CARTESIAN_POINT ( 'NONE',  ( -1.265664690411616068E-16, 66.06698730000000808, 48.55000000109247082 ) ) ;
#9286 = CARTESIAN_POINT ( 'NONE',  ( 2.066987300000001859, 64.85617417291294373, 45.20000000109248361 ) ) ;
#9287 = ORIENTED_EDGE ( 'NONE', *, *, #1469, .T. ) ;
#9288 = ORIENTED_EDGE ( 'NONE', *, *, #13331, .F. ) ;
#9289 = EDGE_CURVE ( 'NONE', #3232, #9967, #12839, .T. ) ;
#9290 = LINE ( 'NONE', #379, #15038 ) ;
#9291 = DIRECTION ( 'NONE',  ( -0.000000000000000000, -1.000000000000000000, -0.000000000000000000 ) ) ;
#9292 = ORIENTED_EDGE ( 'NONE', *, *, #18034, .T. ) ;
#9293 = DIRECTION ( 'NONE',  ( 0.5773502691896255090, -0.8164965809277261455, 0.000000000000000000 ) ) ;
#9294 = DIRECTION ( 'NONE',  ( 1.000000000000000000, 0.000000000000000000, 0.000000000000000000 ) ) ;
#9295 = AXIS2_PLACEMENT_3D ( 'NONE', #16566, #4617, #11744 ) ;
#9296 = CARTESIAN_POINT ( 'NONE',  ( -2.066987300000001415, 63.14382582708705627, 45.00000000109246656 ) ) ;
#9297 = CARTESIAN_POINT ( 'NONE',  ( -9.575581032440641666E-15, 24.22720779386417078, 60.84386001800125143 ) ) ;
#9298 = CARTESIAN_POINT ( 'NONE',  ( -41.00000000000000711, 53.00000000000000711, -18.00000000000000000 ) ) ;
#9299 = EDGE_CURVE ( 'NONE', #5693, #12613, #2354, .T. ) ;
#9300 = EDGE_LOOP ( 'NONE', ( #17041, #5965, #4757, #13823 ) ) ;
#9302 = ORIENTED_EDGE ( 'NONE', *, *, #16594, .T. ) ;
#9301 = VERTEX_POINT ( 'NONE', #7246 ) ;
#9303 = CARTESIAN_POINT ( 'NONE',  ( -9.754982604823348780, -18.99630608921234654, 20.66992750791695954 ) ) ;
#9304 = SURFACE_SIDE_STYLE ('',( #9585 ) ) ;
#9305 = ORIENTED_EDGE ( 'NONE', *, *, #13803, .F. ) ;
#9306 = ORIENTED_EDGE ( 'NONE', *, *, #8104, .F. ) ;
#9307 = CARTESIAN_POINT ( 'NONE',  ( -12.31951028609536536, -25.35725562635139596, 18.48632249208304401 ) ) ;
#9308 = CARTESIAN_POINT ( 'NONE',  ( -15.16482700510258574, -30.99999999999998224, 12.13867750791695421 ) ) ;
#9309 = CARTESIAN_POINT ( 'NONE',  ( -0.8561741729129466183, 61.93301270000000613, 48.10000000109246798 ) ) ;
#9310 = LINE ( 'NONE', #10874, #12207 ) ;
#9311 = ORIENTED_EDGE ( 'NONE', *, *, #5196, .T. ) ;
#9312 = CARTESIAN_POINT ( 'NONE',  ( -17.51566270880201159, -22.35725562635141728, 19.13867750791695954 ) ) ;
#9313 = ORIENTED_EDGE ( 'NONE', *, *, #11452, .T. ) ;
#9314 = LINE ( 'NONE', #6582, #10317 ) ;
#9315 = ORIENTED_EDGE ( 'NONE', *, *, #17103, .T. ) ;
#9316 = PRESENTATION_STYLE_ASSIGNMENT (( #15211 ) ) ;
#9317 = FACE_OUTER_BOUND ( 'NONE', #8069, .T. ) ;
#9318 = CARTESIAN_POINT ( 'NONE',  ( 7.500000000000005329, -38.00000000000000000, 4.500000000000000888 ) ) ;
#9319 = CARTESIAN_POINT ( 'NONE',  ( 44.99999999999997158, 3.000000000000000000, 55.00000000000000000 ) ) ;
#9320 = CARTESIAN_POINT ( 'NONE',  ( 0.8561741729129460632, 66.06698729999999387, 48.50000000109246656 ) ) ;
#9321 = CARTESIAN_POINT ( 'NONE',  ( 0.000000000000000000, 2.357898499370431722, -2.818925648462311528E-15 ) ) ;
#9322 = CARTESIAN_POINT ( 'NONE',  ( -1.171838675107511455E-14, 29.65425233947094341, 56.83102903476761014 ) ) ;
#9323 = CARTESIAN_POINT ( 'NONE',  ( 7.500000000000005329, -38.00000000000000000, 1.500000000000000000 ) ) ;
#9324 = DIRECTION ( 'NONE',  ( -0.000000000000000000, 0.000000000000000000, -1.000000000000000000 ) ) ;
#9325 = EDGE_LOOP ( 'NONE', ( #12329, #9582, #12463, #8593, #6690, #7929, #7514, #18431, #8328, #17816, #4619, #10639, #15683, #14990, #10388, #8651 ) ) ;
#9326 = CARTESIAN_POINT ( 'NONE',  ( -18.53959229564986799, -20.21908421996107563, 14.10742750791695777 ) ) ;
#9327 = CARTESIAN_POINT ( 'NONE',  ( 32.50000000000000000, 0.000000000000000000, -45.00000000000000000 ) ) ;
#9328 = ORIENTED_EDGE ( 'NONE', *, *, #5225, .F. ) ;
#9329 = CARTESIAN_POINT ( 'NONE',  ( -16.17491895705296656, -29.04416526290807710, 19.58007249208303335 ) ) ;
#9330 = CARTESIAN_POINT ( 'NONE',  ( -12.68318583509882380, -26.07549068051207541, 13.45507249208304401 ) ) ;
#9331 = ORIENTED_EDGE ( 'NONE', *, *, #5765, .F. ) ;
#9332 = PLANE ( 'NONE',  #9988 ) ;
#9333 = ORIENTED_EDGE ( 'NONE', *, *, #8035, .F. ) ;
#9334 = CYLINDRICAL_SURFACE ( 'NONE', #299, 4.000000000000001776 ) ;
#9335 = CARTESIAN_POINT ( 'NONE',  ( 3.099999999999998757, 0.000000000000000000, 0.000000000000000000 ) ) ;
#9336 = CONICAL_SURFACE ( 'NONE', #12769, 1.280000000000000027, 1.047197551196593857 ) ;
#9337 = CARTESIAN_POINT ( 'NONE',  ( -3.065533689247737392, -43.60761626555502346, 1.500000000000000000 ) ) ;
#9338 = DIRECTION ( 'NONE',  ( 1.000000000000000000, 0.000000000000000000, 0.000000000000000000 ) ) ;
#9339 = CARTESIAN_POINT ( 'NONE',  ( -25.00000000000000000, 53.00000000000000711, 13.49999999999999822 ) ) ;
#9340 = CARTESIAN_POINT ( 'NONE',  ( 3.000000000000002665, 0.000000000000000000, 2.750000000000000000 ) ) ;
#9341 = EDGE_LOOP ( 'NONE', ( #18268, #16435, #3476, #986 ) ) ;
#9342 = EDGE_CURVE ( 'NONE', #4943, #13549, #19015, .T. ) ;
#9343 = EDGE_CURVE ( 'NONE', #15802, #4327, #11285, .T. ) ;
#9344 = CIRCLE ( 'NONE', #16565, 5.800000000000007816 ) ;
#9345 = DIRECTION ( 'NONE',  ( 6.123233995736766036E-17, -1.000000000000000000, 0.000000000000000000 ) ) ;
#9346 = CARTESIAN_POINT ( 'NONE',  ( -18.78091578003889950, -27.53959229564985378, 12.79492750791695421 ) ) ;
#9347 = CARTESIAN_POINT ( 'NONE',  ( -2.500000000000001776, 64.00000000000000000, 46.90000000218494591 ) ) ;
#9348 = EDGE_CURVE ( 'NONE', #15084, #2159, #1598, .T. ) ;
#9349 = CARTESIAN_POINT ( 'NONE',  ( -12.35725562635140307, -28.24771351637085459, 24.17382249208304046 ) ) ;
#9350 = CARTESIAN_POINT ( 'NONE',  ( -1.040834085586084257E-14, 32.57106781186547551, 49.67157287525382969 ) ) ;
#9351 = CARTESIAN_POINT ( 'NONE',  ( -14.83517299489739649, -18.99999999999997868, 9.513677507916957765 ) ) ;
#9352 = ADVANCED_FACE ( 'NONE', ( #7437, #6074 ), #13404, .T. ) ;
#9353 = CARTESIAN_POINT ( 'NONE',  ( -43.50000000000000000, 2.999000000000001442, 32.50000000000000000 ) ) ;
#9355 = CARTESIAN_POINT ( 'NONE',  ( -13.49542703274178201, -19.04416526290806289, 20.23242750791695954 ) ) ;
#9354 = AXIS2_PLACEMENT_3D ( 'NONE', #19203, #17934, #13401 ) ;
#9356 = DIRECTION ( 'NONE',  ( 0.000000000000000000, 1.000000000000000000, -0.000000000000000000 ) ) ;
#9357 = LINE ( 'NONE', #1926, #10059 ) ;
#9358 = CARTESIAN_POINT ( 'NONE',  ( 3.796994071234847710E-16, 61.93301269999999903, 49.15000000109246514 ) ) ;
#9359 = CARTESIAN_POINT ( 'NONE',  ( 10.71950000000001424, 1.836970198721030181E-16, -1.500000000000000222 ) ) ;
#9360 = CIRCLE ( 'NONE', #17820, 1.599999999999997202 ) ;
#9361 = LINE ( 'NONE', #15351, #17908 ) ;
#9362 = CARTESIAN_POINT ( 'NONE',  ( -25.00000000000000000, 53.00000000000000711, 30.00000000000000000 ) ) ;
#9363 = CARTESIAN_POINT ( 'NONE',  ( 3.796994071234847710E-16, 61.93301269999999903, 47.55000000109247082 ) ) ;
#9364 = CARTESIAN_POINT ( 'NONE',  ( -41.00000000000000711, 53.00000000000000711, 1.500000000000001332 ) ) ;
#9365 = EDGE_LOOP ( 'NONE', ( #14422, #17654, #6676, #11740 ) ) ;
#9366 = VERTEX_POINT ( 'NONE', #5976 ) ;
#9367 = CARTESIAN_POINT ( 'NONE',  ( -8.044165262908093084, -21.95952864787946979, 38.83007249208303335 ) ) ;
#9368 = VECTOR ( 'NONE', #8080, 1000.000000000000000 ) ;
#9369 =( NAMED_UNIT ( * ) PLANE_ANGLE_UNIT ( ) SI_UNIT ( $, .RADIAN. ) );
#9370 = CARTESIAN_POINT ( 'NONE',  ( -12.64274437364858628, -19.58745947852646552, 11.92382249208304223 ) ) ;
#9371 = EDGE_LOOP ( 'NONE', ( #17436, #18243, #1312, #14897 ) ) ;
#9372 = CARTESIAN_POINT ( 'NONE',  ( -11.99999999999999289, -24.16482700510258752, 26.57617750791696309 ) ) ;
#9373 = DIRECTION ( 'NONE',  ( 1.000000000000000000, 0.000000000000000000, 0.000000000000000000 ) ) ;
#9374 = CARTESIAN_POINT ( 'NONE',  ( -8.855408670957602979, -27.35725562635137820, 23.73632249208303691 ) ) ;
#9375 = VECTOR ( 'NONE', #9438, 1000.000000000000000 ) ;
#9376 = AXIS2_PLACEMENT_3D ( 'NONE', #2162, #11254, #13925 ) ;
#9377 = CARTESIAN_POINT ( 'NONE',  ( -1.461580736456473462, 62.53841926354353120, 46.45000000109246940 ) ) ;
#9378 = CARTESIAN_POINT ( 'NONE',  ( -2.066987300000001415, 63.14382582708705627, 48.00000000109246656 ) ) ;
#9379 = VERTEX_POINT ( 'NONE', #9201 ) ;
#9380 = ORIENTED_EDGE ( 'NONE', *, *, #1969, .F. ) ;
#9381 = DIRECTION ( 'NONE',  ( -1.000000000000000000, -0.000000000000000000, -0.000000000000000000 ) ) ;
#9382 = LINE ( 'NONE', #10949, #13857 ) ;
#9383 = VECTOR ( 'NONE', #7450, 1000.000000000000000 ) ;
#9384 = CARTESIAN_POINT ( 'NONE',  ( -2.066987300000001415, 64.00000000000000000, 47.95000000109246940 ) ) ;
#9385 = DIRECTION ( 'NONE',  ( 0.000000000000000000, 1.000000000000000000, 0.000000000000000000 ) ) ;
#9386 = CARTESIAN_POINT ( 'NONE',  ( 3.796994071234847710E-16, 61.93301269999999903, 45.95000000109246940 ) ) ;
#9387 = EDGE_CURVE ( 'NONE', #5878, #6083, #6901, .T. ) ;
#9388 = EDGE_CURVE ( 'NONE', #11814, #262, #9407, .T. ) ;
#9389 = VECTOR ( 'NONE', #9606, 1000.000000000000000 ) ;
#9390 = CARTESIAN_POINT ( 'NONE',  ( -7.999999999999996447, -32.00000000000000711, 0.000000000000000000 ) ) ;
#9391 = EDGE_CURVE ( 'NONE', #834, #6216, #9104, .T. ) ;
#9392 = VECTOR ( 'NONE', #778, 1000.000000000000000 ) ;
#9393 = ORIENTED_EDGE ( 'NONE', *, *, #10563, .T. ) ;
#9395 = ORIENTED_EDGE ( 'NONE', *, *, #15403, .T. ) ;
#9394 = ORIENTED_EDGE ( 'NONE', *, *, #10257, .F. ) ;
#9396 = CARTESIAN_POINT ( 'NONE',  ( -13.28918265808472299, -31.04416526290805933, 32.91992750791695244 ) ) ;
#9397 = ORIENTED_EDGE ( 'NONE', *, *, #15964, .T. ) ;
#9398 = CIRCLE ( 'NONE', #12221, 2.649999999999985700 ) ;
#9399 = ORIENTED_EDGE ( 'NONE', *, *, #5886, .F. ) ;
#9400 = CARTESIAN_POINT ( 'NONE',  ( -11.99999999999999289, -23.83517299489735564, 33.79882249208304756 ) ) ;
#9401 = CARTESIAN_POINT ( 'NONE',  ( -21.95583473709191580, -21.95952864787954084, 18.91992750791695954 ) ) ;
#9402 = AXIS2_PLACEMENT_3D ( 'NONE', #7420, #14873, #7520 ) ;
#9403 = CARTESIAN_POINT ( 'NONE',  ( -0.8561741729129461742, 66.06698730000000808, 47.00000000109247367 ) ) ;
#9404 = CARTESIAN_POINT ( 'NONE',  ( 0.1249999999999895917, 33.66708332270461312, 52.46464466094069934 ) ) ;
#9405 = VERTEX_POINT ( 'NONE', #16460 ) ;
#9406 = CARTESIAN_POINT ( 'NONE',  ( -15.96867458239597326, -26.95583473709190159, 12.35742750791696132 ) ) ;
#9407 = CIRCLE ( 'NONE', #14099, 2.750000000000000000 ) ;
#9408 = EDGE_LOOP ( 'NONE', ( #8345, #19359, #8894, #9875 ) ) ;
#9409 = FACE_OUTER_BOUND ( 'NONE', #8698, .T. ) ;
#9410 = ORIENTED_EDGE ( 'NONE', *, *, #9457, .F. ) ;
#9411 = CARTESIAN_POINT ( 'NONE',  ( 0.2500000000000002220, 5.204748896376250699E-16, -4.250000000000000000 ) ) ;
#9412 = EDGE_CURVE ( 'NONE', #4107, #12989, #18035, .T. ) ;
#9413 = CARTESIAN_POINT ( 'NONE',  ( 0.000000000000000000, 6.000000000000000000, 0.000000000000000000 ) ) ;
#9414 = EDGE_CURVE ( 'NONE', #4427, #12045, #652, .T. ) ;
#9415 = DIRECTION ( 'NONE',  ( 0.000000000000000000, 0.000000000000000000, -1.000000000000000000 ) ) ;
#9416 = CARTESIAN_POINT ( 'NONE',  ( -8.528048594804062077, -42.28611686177728046, 3.000000000000000000 ) ) ;
#9417 = FACE_OUTER_BOUND ( 'NONE', #2964, .T. ) ;
#9418 = CARTESIAN_POINT ( 'NONE',  ( -0.8561741729129461742, 66.06698729999999387, 49.40000000109247225 ) ) ;
#9419 = ITEM_DEFINED_TRANSFORMATION ( 'NONE', 'NONE', #4873,  #1791 ) ;
#9420 = CIRCLE ( 'NONE', #7225, 2.055000000000000160 ) ;
#9421 = DIRECTION ( 'NONE',  ( -0.000000000000000000, -1.000000000000000000, -0.000000000000000000 ) ) ;
#9422 = CARTESIAN_POINT ( 'NONE',  ( -15.20357423236093375, -43.78611686177728046, 1.500000000000000000 ) ) ;
#9423 = VECTOR ( 'NONE', #4532, 1000.000000000000000 ) ;
#9424 = FACE_OUTER_BOUND ( 'NONE', #11838, .T. ) ;
#9425 = CARTESIAN_POINT ( 'NONE',  ( 8.000000000000003553, 0.000000000000000000, 1.500000000000000000 ) ) ;
#9426 = EDGE_LOOP ( 'NONE', ( #13104, #12821 ) ) ;
#9427 = CARTESIAN_POINT ( 'NONE',  ( -18.53959229564986799, -20.21908421996107563, 24.60742750791695954 ) ) ;
#9428 = VECTOR ( 'NONE', #2413, 1000.000000000000000 ) ;
#9429 = LINE ( 'NONE', #17083, #13653 ) ;
#9430 = VERTEX_POINT ( 'NONE', #4611 ) ;
#9431 = PRODUCT_DEFINITION_CONTEXT ( 'detailed design', #18841, 'design' ) ;
#9432 = CARTESIAN_POINT ( 'NONE',  ( -17.35725562635140307, -28.41254052147349185, 14.54882249208304046 ) ) ;
#9433 = VECTOR ( 'NONE', #18027, 1000.000000000000000 ) ;
#9434 = CARTESIAN_POINT ( 'NONE',  ( -13.64274437364857739, -21.31951028609534760, 22.42382249208304401 ) ) ;
#9435 = CARTESIAN_POINT ( 'NONE',  ( -1.909647267044692676, 63.20899822134837365, 45.00000000000000000 ) ) ;
#9436 = VERTEX_POINT ( 'NONE', #16557 ) ;
#9437 = CIRCLE ( 'NONE', #15697, 1.600000000000000311 ) ;
#9438 = DIRECTION ( 'NONE',  ( 0.000000000000000000, 0.000000000000000000, 1.000000000000000000 ) ) ;
#9439 = VERTEX_POINT ( 'NONE', #7743 ) ;
#9440 = EDGE_CURVE ( 'NONE', #18899, #9379, #16939, .T. ) ;
#9441 = DIRECTION ( 'NONE',  ( -1.000000000000000000, -0.000000000000000000, -0.000000000000000000 ) ) ;
#9442 = PLANE ( 'NONE',  #790 ) ;
#9443 =( GEOMETRIC_REPRESENTATION_CONTEXT ( 3 ) GLOBAL_UNCERTAINTY_ASSIGNED_CONTEXT ( ( #5145 ) ) GLOBAL_UNIT_ASSIGNED_CONTEXT ( ( #3280, #10718, #12583 ) ) REPRESENTATION_CONTEXT ( 'NONE', 'WORKASPACE' ) );
#9444 = CARTESIAN_POINT ( 'NONE',  ( -1.035533905932738641, 66.50000000000000000, 45.95000000218494307 ) ) ;
#9445 = DIRECTION ( 'NONE',  ( 0.000000000000000000, -0.000000000000000000, -1.000000000000000000 ) ) ;
#9446 = CARTESIAN_POINT ( 'NONE',  ( -25.00000000000001421, 0.000000000000000000, 42.49999999999997868 ) ) ;
#9447 = CARTESIAN_POINT ( 'NONE',  ( -41.00000000000000711, 110.0000000000000000, 1.500000000000001332 ) ) ;
#9448 = CARTESIAN_POINT ( 'NONE',  ( -25.00000000000000711, 110.0000000000000000, -45.00000000000000000 ) ) ;
#9449 = CIRCLE ( 'NONE', #10371, 5.800000000000007816 ) ;
#9450 = ORIENTED_EDGE ( 'NONE', *, *, #15414, .F. ) ;
#9451 = AXIS2_PLACEMENT_3D ( 'NONE', #1694, #13643, #8323 ) ;
#9452 = CARTESIAN_POINT ( 'NONE',  ( -14.83517299489739649, -18.99999999999997868, 20.01367750791695954 ) ) ;
#9453 = CARTESIAN_POINT ( 'NONE',  ( 1.035533905932739751, 61.50000000000000000, 45.55000000218493739 ) ) ;
#9454 = CARTESIAN_POINT ( 'NONE',  ( -10.58745947852648328, -26.35725562635138530, 18.48632249208304401 ) ) ;
#9455 = EDGE_CURVE ( 'NONE', #14710, #17642, #15094, .T. ) ;
#9456 = LINE ( 'NONE', #9547, #2884 ) ;
#9457 = EDGE_CURVE ( 'NONE', #16369, #1200, #12137, .T. ) ;
#9458 = CARTESIAN_POINT ( 'NONE',  ( -16.17491895705301275, -18.95583473709189803, 19.79492750791695954 ) ) ;
#9459 = CARTESIAN_POINT ( 'NONE',  ( -14.83517299489739649, -18.99999999999997868, 41.01367750791696665 ) ) ;
#9460 = CARTESIAN_POINT ( 'NONE',  ( -18.53959229564986799, -20.21908421996107563, 14.10742750791695777 ) ) ;
#9461 = CARTESIAN_POINT ( 'NONE',  ( -32.50000000000000000, 52.00000000000000711, 15.00000000000000000 ) ) ;
#9462 = CARTESIAN_POINT ( 'NONE',  ( -10.58745947852648328, -26.35725562635138530, 23.73632249208304046 ) ) ;
#9463 = CARTESIAN_POINT ( 'NONE',  ( -1.461580736456473906, 65.46158073645646880, 46.45000000109246940 ) ) ;
#9464 = CARTESIAN_POINT ( 'NONE',  ( 1.035533905932739751, 61.50000000000000000, 49.44999999999999574 ) ) ;
#9465 = DIRECTION ( 'NONE',  ( 0.000000000000000000, 0.7071067811865456854, 0.7071067811865494601 ) ) ;
#9466 = CARTESIAN_POINT ( 'NONE',  ( -25.00000000000000000, 53.00000000000000711, 14.50000000000000000 ) ) ;
#9467 = CARTESIAN_POINT ( 'NONE',  ( 1.461580736456473906, 62.53841926354353120, 47.65000000109247225 ) ) ;
#9468 = CARTESIAN_POINT ( 'NONE',  ( -25.00000000000000000, 110.0000000000000000, -24.49999999999999289 ) ) ;
#9469 = ORIENTED_EDGE ( 'NONE', *, *, #15945, .T. ) ;
#9470 = ORIENTED_EDGE ( 'NONE', *, *, #5920, .T. ) ;
#9471 = CARTESIAN_POINT ( 'NONE',  ( -21.14459132904239169, -20.64274437364858628, 36.86132249208304046 ) ) ;
#9472 = CARTESIAN_POINT ( 'NONE',  ( -11.46040770435015332, -20.21908421996104011, 6.892572492083040459 ) ) ;
#9473 = ORIENTED_EDGE ( 'NONE', *, *, #17059, .F. ) ;
#9474 = CARTESIAN_POINT ( 'NONE',  ( -17.31681416490115311, -26.07549068051209318, 23.29492750791696309 ) ) ;
#9475 = LINE ( 'NONE', #15652, #10501 ) ;
#9476 = EDGE_CURVE ( 'NONE', #14701, #185, #12237, .T. ) ;
#9477 = CARTESIAN_POINT ( 'NONE',  ( -7.999999999999996447, -23.83517299489733432, 12.79882249208303691 ) ) ;
#9478 = CARTESIAN_POINT ( 'NONE',  ( -0.8561741729129465073, 61.93301270000000613, 44.90000000109247225 ) ) ;
#9479 = CARTESIAN_POINT ( 'NONE',  ( 1.461580736456473906, 62.53841926354353120, 47.45000000109246940 ) ) ;
#9480 = ORIENTED_EDGE ( 'NONE', *, *, #19218, .T. ) ;
#9481 = ORIENTED_EDGE ( 'NONE', *, *, #5557, .F. ) ;
#9482 = DIRECTION ( 'NONE',  ( -1.000000000000000000, 0.000000000000000000, 0.000000000000000000 ) ) ;
#9483 = DIRECTION ( 'NONE',  ( -1.000000000000000000, 0.000000000000000000, 0.000000000000000000 ) ) ;
#9484 = PLANE ( 'NONE',  #5924 ) ;
#9485 = CARTESIAN_POINT ( 'NONE',  ( -50.00000000000001421, 3.000000000000000000, 59.99999999999997868 ) ) ;
#9486 = EDGE_CURVE ( 'NONE', #513, #4615, #16611, .T. ) ;
#9487 = FACE_OUTER_BOUND ( 'NONE', #14513, .T. ) ;
#9488 = PLANE ( 'NONE',  #13804 ) ;
#9489 = LINE ( 'NONE', #3331, #17697 ) ;
#9490 = VERTEX_POINT ( 'NONE', #10662 ) ;
#9491 = ORIENTED_EDGE ( 'NONE', *, *, #4490, .F. ) ;
#9492 = CARTESIAN_POINT ( 'NONE',  ( -21.95583473709191580, -21.95952864787954084, 34.66992750791696665 ) ) ;
#9493 = CONTEXT_DEPENDENT_SHAPE_REPRESENTATION ( #11689, #14916 ) ;
#9494 = ORIENTED_EDGE ( 'NONE', *, *, #17300, .F. ) ;
#9495 = EDGE_LOOP ( 'NONE', ( #4218, #7969, #11362, #13919, #3000 ) ) ;
#9496 = CARTESIAN_POINT ( 'NONE',  ( -17.68048971390462754, -22.64274437364856496, 36.86132249208304046 ) ) ;
#9497 = CARTESIAN_POINT ( 'NONE',  ( -20.97976432393977575, -20.35725562635143504, 13.88867750791695599 ) ) ;
#9498 =( BOUNDED_CURVE ( )  B_SPLINE_CURVE ( 2, ( #17403, #4176, #3977, #17222, #10127, #6916, #15931, #18887, #839 ),
 .UNSPECIFIED., .F., .T. ) 
 B_SPLINE_CURVE_WITH_KNOTS ( ( 3, 2, 2, 2, 3 ),
 ( 0.1428571428571429047, 0.1607142857142857262, 0.1785714285714285476, 0.1964285714285713413, 0.2142857142857141350 ),
 .UNSPECIFIED. ) 
 CURVE ( )  GEOMETRIC_REPRESENTATION_ITEM ( )  RATIONAL_B_SPLINE_CURVE ( ( 0.9999999999999997780, 0.9238795325112869605, 1.000000000000000000, 0.9238795325112867385, 1.000000000000000000, 0.9238795325112867385, 1.000000000000000000, 0.9238795325112872936, 0.9999999999999994449 ) ) 
 REPRESENTATION_ITEM ( '' )  );
#9499 = EDGE_CURVE ( 'NONE', #16765, #5967, #10266, .T. ) ;
#9500 = CARTESIAN_POINT ( 'NONE',  ( -2.066987300000001415, 64.85617417291294373, 49.50000000109246656 ) ) ;
#9501 = FACE_OUTER_BOUND ( 'NONE', #16440, .T. ) ;
#9502 = ORIENTED_EDGE ( 'NONE', *, *, #16201, .T. ) ;
#9503 = ADVANCED_FACE ( 'NONE', ( #3228 ), #15189, .F. ) ;
#9504 = CARTESIAN_POINT ( 'NONE',  ( -13.35725562635142794, -21.48433729119796709, 30.95117750791695954 ) ) ;
#9505 = CARTESIAN_POINT ( 'NONE',  ( -2.315774708385978098, 27.98014068711927038, 58.50514068711927251 ) ) ;
#9506 = VERTEX_POINT ( 'NONE', #2829 ) ;
#9507 = CARTESIAN_POINT ( 'NONE',  ( -0.000000000000000000, -52.00000000000000711, 0.000000000000000000 ) ) ;
#9508 = ORIENTED_EDGE ( 'NONE', *, *, #18880, .F. ) ;
#9509 = FACE_OUTER_BOUND ( 'NONE', #17218, .T. ) ;
#9510 = FACE_BOUND ( 'NONE', #2157, .T. ) ;
#9511 = DIRECTION ( 'NONE',  ( 0.000000000000000000, 1.000000000000000000, 1.632680918566406793E-16 ) ) ;
#9512 = FACE_BOUND ( 'NONE', #6890, .T. ) ;
#9513 = LINE ( 'NONE', #8153, #1608 ) ;
#9514 = CONTEXT_DEPENDENT_SHAPE_REPRESENTATION ( #15723, #11432 ) ;
#9515 = CARTESIAN_POINT ( 'NONE',  ( -25.00000000000000000, 53.00000000000000711, -19.00000000000000355 ) ) ;
#9516 = DIRECTION ( 'NONE',  ( 1.000000000000000000, -0.000000000000000000, -0.000000000000000000 ) ) ;
#9517 = DIRECTION ( 'NONE',  ( 0.000000000000000000, -0.000000000000000000, -1.000000000000000000 ) ) ;
#9518 = FACE_OUTER_BOUND ( 'NONE', #16182, .T. ) ;
#9519 = EDGE_LOOP ( 'NONE', ( #2066, #14199, #5986, #3337 ) ) ;
#9520 = CARTESIAN_POINT ( 'NONE',  ( -10.04416526290807710, -25.50457296725819489, 37.29492750791697375 ) ) ;
#9521 = CARTESIAN_POINT ( 'NONE',  ( -15.00000000000000000, 47.00000000000000711, 0.000000000000000000 ) ) ;
#9522 = ORIENTED_EDGE ( 'NONE', *, *, #11376, .F. ) ;
#9523 = VECTOR ( 'NONE', #18777, 1000.000000000000114 ) ;
#9524 = CARTESIAN_POINT ( 'NONE',  ( -12.35725562635140307, -28.24771351637085459, 29.42382249208304401 ) ) ;
#9525 = ADVANCED_FACE ( 'NONE', ( #8812 ), #14799, .T. ) ;
#9526 = CARTESIAN_POINT ( 'NONE',  ( -12.48433729119799196, -22.35725562635139596, 22.86132249208304401 ) ) ;
#9527 = CARTESIAN_POINT ( 'NONE',  ( -14.99999999999999645, 73.00000000000001421, 23.99999999999997868 ) ) ;
#9528 = ORIENTED_EDGE ( 'NONE', *, *, #2771, .T. ) ;
#9529 = DIRECTION ( 'NONE',  ( -0.000000000000000000, -0.000000000000000000, -1.000000000000000000 ) ) ;
#9530 = ORIENTED_EDGE ( 'NONE', *, *, #11765, .T. ) ;
#9531 = PLANE ( 'NONE',  #14371 ) ;
#9532 = EDGE_CURVE ( 'NONE', #15030, #12335, #1468, .T. ) ;
#9533 = CYLINDRICAL_SURFACE ( 'NONE', #11416, 7.000000000000001776 ) ;
#9534 = CARTESIAN_POINT ( 'NONE',  ( -41.00000000000000711, 110.0000000000000000, 13.50000000000000000 ) ) ;
#9535 = CIRCLE ( 'NONE', #11100, 1.500000000000001332 ) ;
#9536 = CARTESIAN_POINT ( 'NONE',  ( 0.000000000000000000, 0.7390083445627193548, -1.280000000000000693 ) ) ;
#9537 = DIRECTION ( 'NONE',  ( 0.000000000000000000, 0.000000000000000000, -1.000000000000000000 ) ) ;
#9538 = DIRECTION ( 'NONE',  ( 0.000000000000000000, 1.000000000000000000, 0.000000000000000000 ) ) ;
#9539 = FACE_OUTER_BOUND ( 'NONE', #8014, .T. ) ;
#9540 = ADVANCED_FACE ( 'NONE', ( #13999 ), #673, .T. ) ;
#9541 = VERTEX_POINT ( 'NONE', #13900 ) ;
#9542 = MECHANICAL_DESIGN_GEOMETRIC_PRESENTATION_REPRESENTATION (  '', ( #15815 ), #3601 ) ;
#9543 = CARTESIAN_POINT ( 'NONE',  ( -16.50457296725820555, -28.95583473709189448, 38.60742750791694533 ) ) ;
#9544 = VECTOR ( 'NONE', #3562, 1000.000000000000000 ) ;
#9545 = CARTESIAN_POINT ( 'NONE',  ( -2.500000000000001776, 65.03553390593273775, 44.45000000218495018 ) ) ;
#9546 = CARTESIAN_POINT ( 'NONE',  ( -9.999999999999994671, -23.83517299489734143, 12.79882249208304046 ) ) ;
#9547 = CARTESIAN_POINT ( 'NONE',  ( 44.99999999999998579, 3.000000000000000000, -56.49999999999998579 ) ) ;
#9548 = EDGE_CURVE ( 'NONE', #15895, #12743, #8227, .T. ) ;
#9549 = CARTESIAN_POINT ( 'NONE',  ( -9.999999999999994671, -24.16482700510257686, 21.32617750791695599 ) ) ;
#9550 = DIRECTION ( 'NONE',  ( -1.000000000000000000, -0.000000000000000000, -0.000000000000000000 ) ) ;
#9551 = CARTESIAN_POINT ( 'NONE',  ( -17.64274437364855430, -28.24771351637087236, 28.32617750791695954 ) ) ;
#9552 = CARTESIAN_POINT ( 'NONE',  ( 44.99999999999998579, 0.000000000000000000, -54.99999999999998579 ) ) ;
#9553 = CARTESIAN_POINT ( 'NONE',  ( -12.64274437364858628, -19.58745947852646552, 27.67382249208304046 ) ) ;
#9554 = CARTESIAN_POINT ( 'NONE',  ( -2.066987300000001859, 64.85617417291294373, 48.10000000109246798 ) ) ;
#9555 = DIRECTION ( 'NONE',  ( 0.000000000000000000, 0.000000000000000000, -1.000000000000000000 ) ) ;
#9556 = AXIS2_PLACEMENT_3D ( 'NONE', #9425, #3257, #9324 ) ;
#9557 = DIRECTION ( 'NONE',  ( 0.000000000000000000, 0.000000000000000000, 1.000000000000000000 ) ) ;
#9558 = AXIS2_PLACEMENT_3D ( 'NONE', #6348, #7616, #16734 ) ;
#9559 = CARTESIAN_POINT ( 'NONE',  ( 1.461580736456473684, 65.46158073645646880, 47.85000000109246798 ) ) ;
#9560 = LINE ( 'NONE', #6638, #15546 ) ;
#9561 = ORIENTED_EDGE ( 'NONE', *, *, #7932, .T. ) ;
#9562 = CARTESIAN_POINT ( 'NONE',  ( -9.020235676060250896, -20.35725562635137820, 33.36132249208304046 ) ) ;
#9563 = CARTESIAN_POINT ( 'NONE',  ( -11.46040770435015332, -20.21908421996104011, 17.39257249208304401 ) ) ;
#9564 = CARTESIAN_POINT ( 'NONE',  ( -15.96867458239597326, -26.95583473709190159, 33.35742750791695954 ) ) ;
#9565 = PLANE ( 'NONE',  #6749 ) ;
#9566 = CARTESIAN_POINT ( 'NONE',  ( -18.35725562635138886, -30.14459132904237393, 14.54882249208303868 ) ) ;
#9567 = VECTOR ( 'NONE', #8228, 1000.000000000000000 ) ;
#9568 = CONICAL_SURFACE ( 'NONE', #7377, 2.055000000000000160, 0.7853981633974712606 ) ;
#9569 = CARTESIAN_POINT ( 'NONE',  ( -0.8561741729129465073, 61.93301270000000613, 46.50000000109247367 ) ) ;
#9570 = CARTESIAN_POINT ( 'NONE',  ( -41.00000000000000711, 113.0000000000000000, 30.00000000000000000 ) ) ;
#9571 = ORIENTED_EDGE ( 'NONE', *, *, #4104, .F. ) ;
#9572 = VERTEX_POINT ( 'NONE', #3702 ) ;
#9573 = CARTESIAN_POINT ( 'NONE',  ( 24.00000000000000000, 0.000000000000000000, -50.00000000000000000 ) ) ;
#9574 = CARTESIAN_POINT ( 'NONE',  ( -24.00000000000000711, 110.0000000000000000, 1.500000000000001332 ) ) ;
#9575 = CARTESIAN_POINT ( 'NONE',  ( 2.066987300000001859, 63.14382582708704916, 48.30000000109247082 ) ) ;
#9576 = CARTESIAN_POINT ( 'NONE',  ( -25.00000000000000711, 53.00000000000000711, 27.50000000000000000 ) ) ;
#9577 = DIRECTION ( 'NONE',  ( 1.000000000000000000, 0.000000000000000000, 0.000000000000000000 ) ) ;
#9578 = CARTESIAN_POINT ( 'NONE',  ( 8.000000000000000000, 68.00000000000000000, 66.99999999999997158 ) ) ;
#9579 = VECTOR ( 'NONE', #17766, 1000.000000000000000 ) ;
#9580 = VECTOR ( 'NONE', #2689, 1000.000000000000000 ) ;
#9581 = DIRECTION ( 'NONE',  ( 0.000000000000000000, -1.000000000000000000, 0.000000000000000000 ) ) ;
#9582 = ORIENTED_EDGE ( 'NONE', *, *, #15990, .T. ) ;
#9583 = VERTEX_POINT ( 'NONE', #8126 ) ;
#9584 = CARTESIAN_POINT ( 'NONE',  ( -21.14459132904236327, -27.35725562635143149, 23.51367750791695599 ) ) ;
#9585 = SURFACE_STYLE_FILL_AREA ( #14004 ) ;
#9586 = ORIENTED_EDGE ( 'NONE', *, *, #11422, .T. ) ;
#9588 = ORIENTED_EDGE ( 'NONE', *, *, #15791, .F. ) ;
#9587 = VERTEX_POINT ( 'NONE', #18617 ) ;
#9589 = CARTESIAN_POINT ( 'NONE',  ( -13.64274437364857739, -21.31951028609534760, 38.17382249208304046 ) ) ;
#9590 = ADVANCED_FACE ( 'NONE', ( #13806 ), #4996, .T. ) ;
#9591 = EDGE_CURVE ( 'NONE', #7475, #4404, #478, .T. ) ;
#9592 = CARTESIAN_POINT ( 'NONE',  ( -7.999999999999996447, -24.16482700510256976, 10.82617750791695599 ) ) ;
#9593 = CARTESIAN_POINT ( 'NONE',  ( 10.71950000000001424, 0.000000000000000000, 1.500000000000000222 ) ) ;
#9594 = CARTESIAN_POINT ( 'NONE',  ( -1.035533905932738641, 66.50000000000000000, 48.35000000218494165 ) ) ;
#9595 = LINE ( 'NONE', #6672, #13448 ) ;
#9596 = ORIENTED_EDGE ( 'NONE', *, *, #2905, .T. ) ;
#9597 = CARTESIAN_POINT ( 'NONE',  ( -16.35725562635142794, -21.31951028609535470, 24.82617750791696309 ) ) ;
#9598 = EDGE_CURVE ( 'NONE', #18891, #3990, #10954, .T. ) ;
#9599 = AXIS2_PLACEMENT_3D ( 'NONE', #16468, #7151, #4416 ) ;
#9600 = LINE ( 'NONE', #9216, #1911 ) ;
#9601 = ORIENTED_EDGE ( 'NONE', *, *, #2055, .T. ) ;
#9602 = AXIS2_PLACEMENT_3D ( 'NONE', #9176, #15161, #7711 ) ;
#9603 = CARTESIAN_POINT ( 'NONE',  ( -43.50000000000000000, 115.0000000000000000, 32.50000000000000000 ) ) ;
#9604 = VERTEX_POINT ( 'NONE', #10758 ) ;
#9605 = CARTESIAN_POINT ( 'NONE',  ( 2.500000000000001776, 64.00000000000000000, 47.99999999999999289 ) ) ;
#9606 = DIRECTION ( 'NONE',  ( -0.000000000000000000, -1.000000000000000000, -0.000000000000000000 ) ) ;
#9607 = CARTESIAN_POINT ( 'NONE',  ( -40.00000000000000711, 53.00000000000000711, -30.99999999999999645 ) ) ;
#9608 = EDGE_CURVE ( 'NONE', #4790, #19215, #12622, .T. ) ;
#9609 = CARTESIAN_POINT ( 'NONE',  ( 2.066987300000001415, 64.00000000000000000, 47.55000000109247082 ) ) ;
#9610 = CARTESIAN_POINT ( 'NONE',  ( -0.8561741729129466183, 61.93301270000000613, 47.50000000109246656 ) ) ;
#9611 = CARTESIAN_POINT ( 'NONE',  ( -44.99999999999998579, 0.000000000000000000, -55.00000000000000000 ) ) ;
#9612 = LINE ( 'NONE', #15598, #4610 ) ;
#9613 = DIRECTION ( 'NONE',  ( 4.898042755699219393E-16, 0.000000000000000000, 1.000000000000000000 ) ) ;
#9614 = ORIENTED_EDGE ( 'NONE', *, *, #11078, .T. ) ;
#9615 = EDGE_CURVE ( 'NONE', #16872, #14967, #3521, .T. ) ;
#9616 = CARTESIAN_POINT ( 'NONE',  ( -11.21908421996108629, -20.46040770435011069, 25.91992750791694888 ) ) ;
#9617 =( BOUNDED_CURVE ( )  B_SPLINE_CURVE ( 2, ( #4969, #18403, #10926, #9464, #15450, #2017, #8567, #10024, #15827 ),
 .UNSPECIFIED., .F., .F. ) 
 B_SPLINE_CURVE_WITH_KNOTS ( ( 3, 2, 2, 2, 3 ),
 ( 0.07142857142857121644, 0.08928571428571414892, 0.1071428571428570675, 0.1250000000000000000, 0.1428571428571429047 ),
 .UNSPECIFIED. ) 
 CURVE ( )  GEOMETRIC_REPRESENTATION_ITEM ( )  RATIONAL_B_SPLINE_CURVE ( ( 1.000000000000000666, 0.9238795325112857393, 1.000000000000000000, 0.9238795325112867385, 1.000000000000000000, 0.9238795325112867385, 1.000000000000000000, 0.9238795325112865164, 1.000000000000000222 ) ) 
 REPRESENTATION_ITEM ( '' )  );
#9618 = DIRECTION ( 'NONE',  ( 1.000000000000000000, -0.000000000000000000, -0.000000000000000000 ) ) ;
#9619 = ORIENTED_EDGE ( 'NONE', *, *, #2516, .T. ) ;
#9620 = CARTESIAN_POINT ( 'NONE',  ( -10.75228648362912232, -21.35725562635138530, 28.11132249208304046 ) ) ;
#9621 = EDGE_CURVE ( 'NONE', #14552, #7196, #8036, .T. ) ;
#9622 = CARTESIAN_POINT ( 'NONE',  ( -12.68318583509882380, -26.07549068051207541, 39.70507249208305467 ) ) ;
#9623 =( NAMED_UNIT ( * ) PLANE_ANGLE_UNIT ( ) SI_UNIT ( $, .RADIAN. ) );
#9624 = ORIENTED_EDGE ( 'NONE', *, *, #11494, .F. ) ;
#9625 = LINE ( 'NONE', #15610, #923 ) ;
#9626 = ORIENTED_EDGE ( 'NONE', *, *, #3470, .F. ) ;
#9627 = LINE ( 'NONE', #6877, #13768 ) ;
#9628 = DIRECTION ( 'NONE',  ( 0.000000000000000000, -0.000000000000000000, 1.000000000000000000 ) ) ;
#9629 = CARTESIAN_POINT ( 'NONE',  ( -3.155775640247338920, -41.39960408384398249, 3.000000000000000000 ) ) ;
#9630 = EDGE_CURVE ( 'NONE', #109, #14590, #4901, .T. ) ;
#9631 = EDGE_CURVE ( 'NONE', #11032, #6116, #11288, .T. ) ;
#9632 = DIRECTION ( 'NONE',  ( 2.220446049250312834E-16, 0.7071067811865455743, 0.7071067811865493491 ) ) ;
#9633 = DIRECTION ( 'NONE',  ( -0.5773502691896228445, 0.8164965809277280329, 0.000000000000000000 ) ) ;
#9634 = ADVANCED_FACE ( 'NONE', ( #4809, #570 ), #9488, .T. ) ;
#9635 = DIRECTION ( 'NONE',  ( -0.000000000000000000, -0.000000000000000000, -1.000000000000000000 ) ) ;
#9636 = LINE ( 'NONE', #12673, #18372 ) ;
#9637 = UNCERTAINTY_MEASURE_WITH_UNIT (LENGTH_MEASURE( 1.000000000000000082E-05 ), #16512, 'distance_accuracy_value', 'NONE');
#9638 = ORIENTED_EDGE ( 'NONE', *, *, #9946, .T. ) ;
#9639 = EDGE_CURVE ( 'NONE', #16741, #2217, #8180, .T. ) ;
#9640 = CARTESIAN_POINT ( 'NONE',  ( -16.17491895705301275, -18.95583473709189803, 25.04492750791695954 ) ) ;
#9641 = CARTESIAN_POINT ( 'NONE',  ( -1.767766952966370209, 65.76776695296638309, 44.40000000218493881 ) ) ;
#9642 = CARTESIAN_POINT ( 'NONE',  ( -18.78091578003892081, -20.46040770435013556, 31.83007249208304401 ) ) ;
#9643 = CYLINDRICAL_SURFACE ( 'NONE', #12189, 2.500000000000001776 ) ;
#9644 = CARTESIAN_POINT ( 'NONE',  ( -19.41254052147348830, -26.35725562635142083, 13.01367750791695777 ) ) ;
#9645 = DIRECTION ( 'NONE',  ( 0.000000000000000000, 1.000000000000000000, 0.000000000000000000 ) ) ;
#9646 = CARTESIAN_POINT ( 'NONE',  ( -10.75228648362910100, -26.64274437364854009, 37.51367750791695954 ) ) ;
#9647 = LINE ( 'NONE', #10828, #1215 ) ;
#9648 = CARTESIAN_POINT ( 'NONE',  ( -20.04416526290809131, -22.82508104294700502, 20.89257249208304046 ) ) ;
#9649 = EDGE_CURVE ( 'NONE', #12041, #1793, #5183, .T. ) ;
#9650 = CARTESIAN_POINT ( 'NONE',  ( 2.500000000000001776, 65.03553390593273775, 48.85000000000000142 ) ) ;
#9651 = DIRECTION ( 'NONE',  ( 0.000000000000000000, 0.000000000000000000, -1.000000000000000000 ) ) ;
#9652 = CARTESIAN_POINT ( 'NONE',  ( 1.035533905932738197, 66.50000000000000000, 48.25000000218494733 ) ) ;
#9653 = CARTESIAN_POINT ( 'NONE',  ( -2.066987300000001859, 64.85617417291294373, 47.30000000109247082 ) ) ;
#9654 = DIRECTION ( 'NONE',  ( 1.000000000000000000, -0.000000000000000000, -0.000000000000000000 ) ) ;
#9655 = VECTOR ( 'NONE', #6145, 1000.000000000000000 ) ;
#9656 = ORIENTED_EDGE ( 'NONE', *, *, #13067, .T. ) ;
#9657 = CARTESIAN_POINT ( 'NONE',  ( -14.83517299489734853, -30.99999999999998224, 29.86132249208304046 ) ) ;
#9658 = CARTESIAN_POINT ( 'NONE',  ( -1.461580736456473906, 65.46158073645646880, 44.65000000109246514 ) ) ;
#9659 = CARTESIAN_POINT ( 'NONE',  ( -14.83517299489738761, -20.99999999999997513, 25.26367750791696309 ) ) ;
#9660 = PRODUCT_RELATED_PRODUCT_CATEGORY ( 'part', '', ( #10187 ) ) ;
#9661 = FACE_OUTER_BOUND ( 'NONE', #14391, .T. ) ;
#9662 = CARTESIAN_POINT ( 'NONE',  ( -21.99999999999999289, -24.16482700510262305, 36.42382249208304756 ) ) ;
#9663 = VECTOR ( 'NONE', #9073, 1000.000000000000000 ) ;
#9664 = CARTESIAN_POINT ( 'NONE',  ( -2.066987300000001415, 63.14382582708705627, 45.60000000109246088 ) ) ;
#9665 = ORIENTED_EDGE ( 'NONE', *, *, #19333, .F. ) ;
#9666 = ORIENTED_EDGE ( 'NONE', *, *, #3097, .T. ) ;
#9667 = AXIS2_PLACEMENT_3D ( 'NONE', #9552, #3677, #12597 ) ;
#9668 = CARTESIAN_POINT ( 'NONE',  ( 1.300000000000000044, 0.7390083445627224634, 1.279999999999999138 ) ) ;
#9669 = CARTESIAN_POINT ( 'NONE',  ( -5.800000000000006928, 29.65425233947099315, 56.47747564417430510 ) ) ;
#9670 = EDGE_CURVE ( 'NONE', #76, #19248, #5097, .T. ) ;
#9671 = CARTESIAN_POINT ( 'NONE',  ( -1.461580736456473906, 65.46158073645646880, 45.45000000109246940 ) ) ;
#9672 = DIRECTION ( 'NONE',  ( -0.000000000000000000, -1.000000000000000000, -0.000000000000000000 ) ) ;
#9673 = CARTESIAN_POINT ( 'NONE',  ( 2.500000000000000000, 2.357898499370431722, -2.818925648462311528E-15 ) ) ;
#9674 = DIRECTION ( 'NONE',  ( 0.000000000000000000, 0.7071067811865494601, -0.7071067811865456854 ) ) ;
#9675 = VECTOR ( 'NONE', #11833, 1000.000000000000000 ) ;
#9676 = DIRECTION ( 'NONE',  ( 0.000000000000000000, 0.000000000000000000, 1.000000000000000000 ) ) ;
#9677 = ORIENTED_EDGE ( 'NONE', *, *, #12084, .F. ) ;
#9678 = ORIENTED_EDGE ( 'NONE', *, *, #9615, .F. ) ;
#9679 = CARTESIAN_POINT ( 'NONE',  ( -16.71081734191527346, -16.95583473709190159, 25.04492750791695599 ) ) ;
#9680 = VECTOR ( 'NONE', #4350, 1000.000000000000000 ) ;
#9681 = ORIENTED_EDGE ( 'NONE', *, *, #19333, .T. ) ;
#9682 = VECTOR ( 'NONE', #4994, 1000.000000000000000 ) ;
#9684 = ORIENTED_EDGE ( 'NONE', *, *, #477, .T. ) ;
#9683 = VERTEX_POINT ( 'NONE', #1954 ) ;
#9685 = CARTESIAN_POINT ( 'NONE',  ( -17.68048971390462754, -22.64274437364856496, 26.36132249208304401 ) ) ;
#9686 = CARTESIAN_POINT ( 'NONE',  ( -11.64274437364854187, -30.14459132904234195, 16.95117750791695954 ) ) ;
#9687 = CARTESIAN_POINT ( 'NONE',  ( -50.00000000000002132, 30.00000000000000355, 37.49999999999996447 ) ) ;
#9688 = CARTESIAN_POINT ( 'NONE',  ( 1.035533905932739751, 61.50000000000000000, 46.35000000218493454 ) ) ;
#9689 = CARTESIAN_POINT ( 'NONE',  ( -37.50000000000002132, 0.000000000000000000, 47.49999999999997868 ) ) ;
#9690 = VERTEX_POINT ( 'NONE', #9578 ) ;
#9691 = CARTESIAN_POINT ( 'NONE',  ( -13.35725562635142794, -21.48433729119796709, 25.70117750791695954 ) ) ;
#9692 = VECTOR ( 'NONE', #7783, 1000.000000000000000 ) ;
#9693 = CARTESIAN_POINT ( 'NONE',  ( 44.99999999999998579, 6.000000000000000000, -56.49999999999998579 ) ) ;
#9694 = ORIENTED_EDGE ( 'NONE', *, *, #18759, .F. ) ;
#9695 = LINE ( 'NONE', #14489, #7842 ) ;
#9696 = VERTEX_POINT ( 'NONE', #9390 ) ;
#9697 = APPLICATION_CONTEXT ( 'automotive_design' ) ;
#9698 = DIRECTION ( 'NONE',  ( 0.000000000000000000, 0.7071067811865456854, 0.7071067811865493491 ) ) ;
#9699 = CARTESIAN_POINT ( 'NONE',  ( 1.767766984964166399, 65.76776692096858312, 45.00000000000000000 ) ) ;
#9700 = VECTOR ( 'NONE', #18639, 1000.000000000000114 ) ;
#9701 = CARTESIAN_POINT ( 'NONE',  ( -2.066987300000001415, 64.00000000000000000, 49.55000000109247082 ) ) ;
#9702 = CARTESIAN_POINT ( 'NONE',  ( -0.8561741729129466183, 61.93301270000000613, 49.10000000109246088 ) ) ;
#9703 = CARTESIAN_POINT ( 'NONE',  ( -41.00000000000000711, 53.00000000000000711, 8.000000000000000000 ) ) ;
#9704 = FACE_OUTER_BOUND ( 'NONE', #15359, .T. ) ;
#9705 = CIRCLE ( 'NONE', #18780, 2.499999999999998668 ) ;
#9706 = DIRECTION ( 'NONE',  ( 2.220446049250312834E-16, 0.7071067811865455743, 0.7071067811865493491 ) ) ;
#9707 = ORIENTED_EDGE ( 'NONE', *, *, #2758, .F. ) ;
#9708 = VERTEX_POINT ( 'NONE', #9297 ) ;
#9709 = CARTESIAN_POINT ( 'NONE',  ( -17.64274437364855430, -28.24771351637087236, 28.32617750791695954 ) ) ;
#9710 = LINE ( 'NONE', #8621, #17415 ) ;
#9711 = VERTEX_POINT ( 'NONE', #15573 ) ;
#9712 = CIRCLE ( 'NONE', #8453, 2.500000000000002220 ) ;
#9713 = CARTESIAN_POINT ( 'NONE',  ( -13.82508104294702100, -18.95583473709188382, 32.70507249208304046 ) ) ;
#9714 = ADVANCED_FACE ( 'NONE', ( #2140 ), #14098, .T. ) ;
#9715 = AXIS2_PLACEMENT_3D ( 'NONE', #877, #11449, #5775 ) ;
#9716 = DIRECTION ( 'NONE',  ( 1.000000000000000000, -0.000000000000000000, -0.000000000000000000 ) ) ;
#9717 = CARTESIAN_POINT ( 'NONE',  ( -16.35725562635141372, -26.68048971390461332, 35.54882249208304046 ) ) ;
#9718 = EDGE_LOOP ( 'NONE', ( #4591, #1071, #8818, #9219, #15872 ) ) ;
#9719 = CIRCLE ( 'NONE', #15352, 1.678500596222258556 ) ;
#9720 = CARTESIAN_POINT ( 'NONE',  ( -25.00000000000000000, 110.0000000000000000, 30.00000000000000000 ) ) ;
#9721 = ORIENTED_EDGE ( 'NONE', *, *, #17193, .T. ) ;
#9722 = DIRECTION ( 'NONE',  ( 0.000000000000000000, 0.000000000000000000, -1.000000000000000000 ) ) ;
#9723 = FACE_OUTER_BOUND ( 'NONE', #9894, .T. ) ;
#9724 = LINE ( 'NONE', #7891, #16319 ) ;
#9725 = ADVANCED_FACE ( 'NONE', ( #13082 ), #5459, .F. ) ;
#9726 = AXIS2_PLACEMENT_3D ( 'NONE', #1852, #6656, #9674 ) ;
#9727 = CARTESIAN_POINT ( 'NONE',  ( -12.50000000000000000, -35.50000000000000000, 1.500000000000000000 ) ) ;
#9728 = LINE ( 'NONE', #695, #18212 ) ;
#9729 = LINE ( 'NONE', #2377, #19286 ) ;
#9730 = CYLINDRICAL_SURFACE ( 'NONE', #18384, 2.500000000000002220 ) ;
#9731 = AXIS2_PLACEMENT_3D ( 'NONE', #14814, #17651, #11754 ) ;
#9732 = EDGE_LOOP ( 'NONE', ( #6931, #4109, #4313, #7284 ) ) ;
#9733 = VECTOR ( 'NONE', #12062, 1000.000000000000000 ) ;
#9734 = CARTESIAN_POINT ( 'NONE',  ( -17.35725562635144215, -19.58745947852648683, 30.07617750791695599 ) ) ;
#9735 = CARTESIAN_POINT ( 'NONE',  ( 3.796994071234847710E-16, 61.93301269999999903, 46.55000000109247082 ) ) ;
#9736 = CARTESIAN_POINT ( 'NONE',  ( -12.64274437364858628, -19.58745947852646552, 38.17382249208304046 ) ) ;
#9737 = VECTOR ( 'NONE', #13830, 1000.000000000000000 ) ;
#9738 = EDGE_CURVE ( 'NONE', #2289, #9106, #11420, .T. ) ;
#9739 = EDGE_CURVE ( 'NONE', #16140, #17064, #7020, .T. ) ;
#9740 = CARTESIAN_POINT ( 'NONE',  ( 2.500000000000001776, 64.00000000000000000, 46.50000000218494733 ) ) ;
#9741 = CARTESIAN_POINT ( 'NONE',  ( -16.50457296725820555, -28.95583473709189448, 33.35742750791695954 ) ) ;
#9742 = EDGE_CURVE ( 'NONE', #3695, #17145, #11599, .T. ) ;
#9743 = VECTOR ( 'NONE', #18983, 1000.000000000000000 ) ;
#9744 = FACE_OUTER_BOUND ( 'NONE', #6272, .T. ) ;
#9745 = CARTESIAN_POINT ( 'NONE',  ( -16.50457296725820555, -28.95583473709189803, 38.60742750791695954 ) ) ;
#9746 = DIRECTION ( 'NONE',  ( 1.000000000000000000, -0.000000000000000000, -0.000000000000000000 ) ) ;
#9747 = CARTESIAN_POINT ( 'NONE',  ( -13.49542703274174116, -28.95583473709188738, 24.39257249208304046 ) ) ;
#9748 = CARTESIAN_POINT ( 'NONE',  ( 1.035533905932739751, 61.50000000000000000, 49.44999999999999574 ) ) ;
#9749 = LINE ( 'NONE', #14257, #16549 ) ;
#9750 = VECTOR ( 'NONE', #8837, 1000.000000000000000 ) ;
#9751 = CARTESIAN_POINT ( 'NONE',  ( -1.040834085586084257E-14, 33.84386001800125143, 52.64142135623732344 ) ) ;
#9752 = CARTESIAN_POINT ( 'NONE',  ( 1.461580736456473684, 65.46158073645646880, 45.45000000109246940 ) ) ;
#9753 = CARTESIAN_POINT ( 'NONE',  ( -9.673552776372430100E-15, 27.62132034355963839, 46.13603896932106352 ) ) ;
#9754 = VECTOR ( 'NONE', #10158, 1000.000000000000000 ) ;
#9755 = EDGE_LOOP ( 'NONE', ( #122, #7947, #10568, #14285 ) ) ;
#9756 = CARTESIAN_POINT ( 'NONE',  ( -1.461580736456473462, 62.53841926354353120, 45.65000000109247225 ) ) ;
#9757 = CARTESIAN_POINT ( 'NONE',  ( -15.63902057219076269, -20.95583473709189448, 35.54492750791696665 ) ) ;
#9758 = DIRECTION ( 'NONE',  ( 0.000000000000000000, 0.000000000000000000, 1.000000000000000000 ) ) ;
#9759 = CARTESIAN_POINT ( 'NONE',  ( -13.28918265808478694, -16.95583473709189093, 32.70507249208304756 ) ) ;
#9760 = EDGE_CURVE ( 'NONE', #10640, #17050, #19082, .T. ) ;
#9761 = CARTESIAN_POINT ( 'NONE',  ( -1.265664690411616068E-16, 66.06698730000000808, 45.35000000109246798 ) ) ;
#9762 = ORIENTED_EDGE ( 'NONE', *, *, #14302, .T. ) ;
#9763 = VECTOR ( 'NONE', #7904, 1000.000000000000000 ) ;
#9764 = PLANE ( 'NONE',  #17848 ) ;
#9765 = CARTESIAN_POINT ( 'NONE',  ( 24.99999999999998579, 107.3545527679194436, 47.49999999999997868 ) ) ;
#9766 = CARTESIAN_POINT ( 'NONE',  ( 0.7910017786515960436, 62.09035273295529578, 44.99999999999998579 ) ) ;
#9767 = LINE ( 'NONE', #13802, #18775 ) ;
#9768 = DIRECTION ( 'NONE',  ( 0.000000000000000000, 0.7071067811865456854, 0.7071067811865493491 ) ) ;
#9769 = CARTESIAN_POINT ( 'NONE',  ( -1.035533905932738863, 61.50000000000000000, 48.54999999999999716 ) ) ;
#9770 = CARTESIAN_POINT ( 'NONE',  ( -1.485306817036799787, -32.50000000000000711, 1.500000000000000444 ) ) ;
#9771 = ORIENTED_EDGE ( 'NONE', *, *, #16728, .F. ) ;
#9772 = ORIENTED_EDGE ( 'NONE', *, *, #14705, .F. ) ;
#9773 = CARTESIAN_POINT ( 'NONE',  ( -7.955834737091916686, -22.28918265808470522, 36.85742750791695244 ) ) ;
#9774 = SURFACE_SIDE_STYLE ('',( #9951 ) ) ;
#9775 = ORIENTED_EDGE ( 'NONE', *, *, #6928, .F. ) ;
#9777 = VERTEX_POINT ( 'NONE', #5373 ) ;
#9776 = ORIENTED_EDGE ( 'NONE', *, *, #4394, .T. ) ;
#9778 = EDGE_CURVE ( 'NONE', #8350, #14552, #11229, .T. ) ;
#9779 = CARTESIAN_POINT ( 'NONE',  ( -14.03132541760400009, -26.95583473709189448, 34.89257249208305467 ) ) ;
#9780 = CARTESIAN_POINT ( 'NONE',  ( -15.16482700510258574, -30.99999999999998224, 33.13867750791695954 ) ) ;
#9781 = FACE_BOUND ( 'NONE', #10507, .T. ) ;
#9782 = CARTESIAN_POINT ( 'NONE',  ( -1.767766952966369765, 62.23223304703363112, 46.20000000218494307 ) ) ;
#9783 = LINE ( 'NONE', #12912, #13136 ) ;
#9784 = ORIENTED_EDGE ( 'NONE', *, *, #10324, .T. ) ;
#9785 = CYLINDRICAL_SURFACE ( 'NONE', #3475, 2.500000000000002220 ) ;
#9786 = EDGE_LOOP ( 'NONE', ( #6874, #4745, #13720, #9393, #10975, #1488, #3833, #14405 ) ) ;
#9787 = DIRECTION ( 'NONE',  ( 0.000000000000000000, 0.000000000000000000, -1.000000000000000000 ) ) ;
#9788 = ORIENTED_EDGE ( 'NONE', *, *, #2832, .F. ) ;
#9789 = CARTESIAN_POINT ( 'NONE',  ( -1.654487106972472477, 62.73153187564108180, 45.00000000000000000 ) ) ;
#9790 = EDGE_CURVE ( 'NONE', #895, #16765, #1235, .T. ) ;
#9791 = DIRECTION ( 'NONE',  ( -2.973811673103096679E-16, 0.000000000000000000, 1.000000000000000000 ) ) ;
#9792 = DIRECTION ( 'NONE',  ( 0.000000000000000000, -1.000000000000000000, 0.000000000000000000 ) ) ;
#9793 = CARTESIAN_POINT ( 'NONE',  ( 3.796994071234847710E-16, 61.93301269999999903, 45.75000000109247367 ) ) ;
#9794 = CARTESIAN_POINT ( 'NONE',  ( -1.265664690411616068E-16, 66.06698730000000808, 47.95000000109246940 ) ) ;
#9795 = DIRECTION ( 'NONE',  ( 1.000000000000000000, 0.000000000000000000, 0.000000000000000000 ) ) ;
#9796 = CARTESIAN_POINT ( 'NONE',  ( 2.500000000000001776, 64.00000000000000000, 49.60000000000000142 ) ) ;
#9797 = DIRECTION ( 'NONE',  ( -1.000000000000000000, 0.000000000000000000, 4.898042755699219393E-16 ) ) ;
#9798 = ORIENTED_EDGE ( 'NONE', *, *, #8070, .T. ) ;
#9799 = ORIENTED_EDGE ( 'NONE', *, *, #13664, .T. ) ;
#9800 = CARTESIAN_POINT ( 'NONE',  ( -14.83517299489739649, -18.99999999999997868, 25.26367750791695599 ) ) ;
#9801 = CARTESIAN_POINT ( 'NONE',  ( 0.000000000000000000, 0.000000000000000000, 0.000000000000000000 ) ) ;
#9802 = ORIENTED_EDGE ( 'NONE', *, *, #14757, .T. ) ;
#9803 = EDGE_CURVE ( 'NONE', #16441, #15290, #3497, .T. ) ;
#9804 = CARTESIAN_POINT ( 'NONE',  ( -19.99999999999999645, -24.16482700510261949, 36.42382249208304046 ) ) ;
#9805 = LINE ( 'NONE', #10085, #8719 ) ;
#9806 = CARTESIAN_POINT ( 'NONE',  ( -12.48433729119799196, -22.35725562635139596, 28.11132249208304401 ) ) ;
#9807 = CARTESIAN_POINT ( 'NONE',  ( 2.500000000000001776, 64.00000000000000000, 34.99999999999999289 ) ) ;
#9808 = ORIENTED_EDGE ( 'NONE', *, *, #1110, .F. ) ;
#9809 = DIRECTION ( 'NONE',  ( 0.000000000000000000, 0.000000000000000000, -1.000000000000000000 ) ) ;
#9810 = VERTEX_POINT ( 'NONE', #5653 ) ;
#9811 = CARTESIAN_POINT ( 'NONE',  ( -4.999999999999980460, 68.00000000000000000, 69.99999999999998579 ) ) ;
#9812 = CARTESIAN_POINT ( 'NONE',  ( -45.00000000000000000, 0.000000000000000000, 54.99999999999998579 ) ) ;
#9813 = DIRECTION ( 'NONE',  ( 1.000000000000000000, -0.000000000000000000, -0.000000000000000000 ) ) ;
#9814 = FACE_BOUND ( 'NONE', #14601, .T. ) ;
#9815 = LINE ( 'NONE', #15810, #5371 ) ;
#9816 = LINE ( 'NONE', #2287, #11144 ) ;
#9817 = CARTESIAN_POINT ( 'NONE',  ( 5.799999999999985612, 29.47747564417429444, 56.65425233947099315 ) ) ;
#9818 = EDGE_LOOP ( 'NONE', ( #17445, #16273 ) ) ;
#9819 = ORIENTED_EDGE ( 'NONE', *, *, #15513, .F. ) ;
#9820 = CARTESIAN_POINT ( 'NONE',  ( -15.16482700510259640, -28.99999999999998224, 33.13867750791696665 ) ) ;
#9821 = CARTESIAN_POINT ( 'NONE',  ( -2.066987300000001859, 64.85617417291294373, 48.70000000109247651 ) ) ;
#9822 = EDGE_CURVE ( 'NONE', #14706, #535, #18709, .T. ) ;
#9823 = EDGE_CURVE ( 'NONE', #3035, #12614, #14739, .T. ) ;
#9824 = CARTESIAN_POINT ( 'NONE',  ( -10.04416526290808953, -22.49542703274172695, 33.58007249208304046 ) ) ;
#9825 = VECTOR ( 'NONE', #18943, 1000.000000000000000 ) ;
#9826 = CARTESIAN_POINT ( 'NONE',  ( -8.528048594804062077, -45.28611686177728046, 1.500000000000000000 ) ) ;
#9827 = CARTESIAN_POINT ( 'NONE',  ( -19.95583473709191580, -22.49542703274176603, 34.66992750791694533 ) ) ;
#9828 = ADVANCED_FACE ( 'NONE', ( #14472 ), #12987, .F. ) ;
#9829 = DIRECTION ( 'NONE',  ( -0.000000000000000000, -0.000000000000000000, -1.000000000000000000 ) ) ;
#9830 = CARTESIAN_POINT ( 'NONE',  ( -19.24771351637089367, -21.35725562635142438, 34.88867750791696665 ) ) ;
#9831 = CARTESIAN_POINT ( 'NONE',  ( -41.00000000000000711, 110.0000000000000000, -37.50000000000000711 ) ) ;
#9832 = CARTESIAN_POINT ( 'NONE',  ( -10.04416526290808598, -22.49542703274172695, 23.08007249208303691 ) ) ;
#9833 = CARTESIAN_POINT ( 'NONE',  ( -0.8561741729129465073, 61.93301270000000613, 45.90000000109247225 ) ) ;
#9834 = LINE ( 'NONE', #17212, #17471 ) ;
#9835 = CARTESIAN_POINT ( 'NONE',  ( -40.00000000000000711, 113.0000000000000000, -19.00000000000000355 ) ) ;
#9836 = CARTESIAN_POINT ( 'NONE',  ( -0.8561741729129461742, 66.06698729999999387, 45.60000000109246088 ) ) ;
#9837 = LINE ( 'NONE', #14455, #16481 ) ;
#9838 = EDGE_CURVE ( 'NONE', #8266, #13522, #17885, .T. ) ;
#9839 = VECTOR ( 'NONE', #12872, 1000.000000000000000 ) ;
#9840 = ORIENTED_EDGE ( 'NONE', *, *, #10010, .F. ) ;
#9841 = EDGE_CURVE ( 'NONE', #10684, #11368, #3889, .T. ) ;
#9842 = CARTESIAN_POINT ( 'NONE',  ( -0.9999999999999945599, -36.00000000000000711, 9.500000000000001776 ) ) ;
#9843 = CARTESIAN_POINT ( 'NONE',  ( -17.31681416490115311, -26.07549068051209318, 39.04492750791695954 ) ) ;
#9844 = CYLINDRICAL_SURFACE ( 'NONE', #19165, 1.599999999999997202 ) ;
#9845 = CARTESIAN_POINT ( 'NONE',  ( -16.71081734191520596, -31.04416526290808065, 30.08007249208304046 ) ) ;
#9846 = CARTESIAN_POINT ( 'NONE',  ( -2.066987300000001859, 64.85617417291294373, 47.30000000109247082 ) ) ;
#9847 = EDGE_CURVE ( 'NONE', #18913, #6733, #11617, .T. ) ;
#9848 = VERTEX_POINT ( 'NONE', #8397 ) ;
#9849 = AXIS2_PLACEMENT_3D ( 'NONE', #12297, #4858, #3186 ) ;
#9850 = DIRECTION ( 'NONE',  ( 0.000000000000000000, 0.000000000000000000, 1.000000000000000000 ) ) ;
#9851 = LINE ( 'NONE', #19075, #366 ) ;
#9852 = VECTOR ( 'NONE', #10093, 1000.000000000000000 ) ;
#9853 = DIRECTION ( 'NONE',  ( 0.000000000000000000, 1.000000000000000000, -1.320393690296331133E-15 ) ) ;
#9854 = DIRECTION ( 'NONE',  ( 0.000000000000000000, -0.7071067811865455743, -0.7071067811865495711 ) ) ;
#9855 = CARTESIAN_POINT ( 'NONE',  ( -2.500000000000001776, 64.00000000000000000, 47.59999999999999432 ) ) ;
#9856 = CARTESIAN_POINT ( 'NONE',  ( -2.499999999999984013, 62.96446609406724804, 48.45000000000000284 ) ) ;
#9857 = EDGE_CURVE ( 'NONE', #908, #17649, #17609, .T. ) ;
#9858 = EDGE_CURVE ( 'NONE', #9098, #8045, #16044, .T. ) ;
#9859 = FACE_OUTER_BOUND ( 'NONE', #19201, .T. ) ;
#9860 = ORIENTED_EDGE ( 'NONE', *, *, #2220, .T. ) ;
#9861 = VERTEX_POINT ( 'NONE', #14771 ) ;
#9862 = CARTESIAN_POINT ( 'NONE',  ( -21.14459132904236327, -27.35725562635143149, 39.26367750791695244 ) ) ;
#9863 = AXIS2_PLACEMENT_3D ( 'NONE', #12365, #1984, #13935 ) ;
#9864 = ORIENTED_EDGE ( 'NONE', *, *, #18143, .F. ) ;
#9865 = VECTOR ( 'NONE', #1830, 1000.000000000000000 ) ;
#9867 = ORIENTED_EDGE ( 'NONE', *, *, #7576, .T. ) ;
#9866 = ORIENTED_EDGE ( 'NONE', *, *, #7976, .T. ) ;
#9868 = PRODUCT_DEFINITION_SHAPE ( 'NONE', 'NONE',  #19411 ) ;
#9869 = CARTESIAN_POINT ( 'NONE',  ( -14.83517299489738761, -20.99999999999997513, 4.263677507916960430 ) ) ;
#9870 = EDGE_CURVE ( 'NONE', #13549, #10345, #14134, .T. ) ;
#9871 = CARTESIAN_POINT ( 'NONE',  ( -9.020235676060220698, -27.64274437364852588, 27.01367750791695599 ) ) ;
#9872 = FACE_OUTER_BOUND ( 'NONE', #18837, .T. ) ;
#9873 = CARTESIAN_POINT ( 'NONE',  ( 1.767766952966370653, 62.23223304703363112, 48.80000000218494449 ) ) ;
#9874 = CARTESIAN_POINT ( 'NONE',  ( -6.528048594804060301, -45.28611686177728046, 3.000000000000000000 ) ) ;
#9875 = ORIENTED_EDGE ( 'NONE', *, *, #2645, .T. ) ;
#9876 = DIRECTION ( 'NONE',  ( 0.000000000000000000, -0.5000000000000011102, -0.8660254037844379305 ) ) ;
#9877 = ORIENTED_EDGE ( 'NONE', *, *, #5730, .T. ) ;
#9878 = CARTESIAN_POINT ( 'NONE',  ( -43.50000000000000000, 2.999000000000001442, 32.50000000000000000 ) ) ;
#9879 = ORIENTED_EDGE ( 'NONE', *, *, #2327, .F. ) ;
#9880 = CARTESIAN_POINT ( 'NONE',  ( 2.500000000000000000, 0.000000000000000000, 0.000000000000000000 ) ) ;
#9881 = LINE ( 'NONE', #19106, #17813 ) ;
#9882 = CARTESIAN_POINT ( 'NONE',  ( 11.00000000000000355, 1.493456771560197319E-16, -1.219500000000000028 ) ) ;
#9883 = VECTOR ( 'NONE', #14774, 1000.000000000000000 ) ;
#9884 = CARTESIAN_POINT ( 'NONE',  ( -1.265664690411616068E-16, 66.06698730000000808, 46.95000000109246940 ) ) ;
#9885 = AXIS2_PLACEMENT_3D ( 'NONE', #15531, #624, #2103 ) ;
#9886 = EDGE_CURVE ( 'NONE', #17827, #7050, #19182, .T. ) ;
#9887 = FACE_OUTER_BOUND ( 'NONE', #11517, .T. ) ;
#9888 = DIRECTION ( 'NONE',  ( 0.000000000000000000, 0.000000000000000000, -1.000000000000000000 ) ) ;
#9889 = FACE_OUTER_BOUND ( 'NONE', #4028, .T. ) ;
#9890 = VERTEX_POINT ( 'NONE', #16231 ) ;
#9891 = EDGE_LOOP ( 'NONE', ( #18255, #16840, #10056, #6497 ) ) ;
#9892 = CARTESIAN_POINT ( 'NONE',  ( -22.04416526290807710, -25.71081734191525925, 7.982427507916956877 ) ) ;
#9893 = CARTESIAN_POINT ( 'NONE',  ( -14.99999999999999645, 73.00000000000001421, 23.99999999999997868 ) ) ;
#9894 = EDGE_LOOP ( 'NONE', ( #5464, #4923, #7051, #9205 ) ) ;
#9895 = CARTESIAN_POINT ( 'NONE',  ( -16.17491895705296656, -29.04416526290807710, 30.08007249208304401 ) ) ;
#9896 = VECTOR ( 'NONE', #3161, 1000.000000000000000 ) ;
#9897 = VECTOR ( 'NONE', #2954, 1000.000000000000000 ) ;
#9898 = CARTESIAN_POINT ( 'NONE',  ( -1.767766952966370209, 65.76776695296638309, 45.09999999999999432 ) ) ;
#9899 = ORIENTED_EDGE ( 'NONE', *, *, #6546, .F. ) ;
#9900 = CARTESIAN_POINT ( 'NONE',  ( -15.16482700510262482, -20.99999999999997513, 27.23632249208304046 ) ) ;
#9901 = CARTESIAN_POINT ( 'NONE',  ( 41.00000000000000000, 52.00000000000000711, 30.00000000000000000 ) ) ;
#9902 = ORIENTED_EDGE ( 'NONE', *, *, #6772, .T. ) ;
#9903 = ORIENTED_EDGE ( 'NONE', *, *, #848, .F. ) ;
#9904 = CARTESIAN_POINT ( 'NONE',  ( 11.00000000000000355, 1.219500000000000028, 0.000000000000000000 ) ) ;
#9905 = CARTESIAN_POINT ( 'NONE',  ( -2.500000000000001776, 64.00000000000000000, 45.30000000218493739 ) ) ;
#9906 = DIRECTION ( 'NONE',  ( -0.000000000000000000, -0.000000000000000000, -1.000000000000000000 ) ) ;
#9907 = VECTOR ( 'NONE', #1075, 1000.000000000000000 ) ;
#9908 = CARTESIAN_POINT ( 'NONE',  ( -16.50457296725820555, -28.95583473709189448, 33.35742750791695954 ) ) ;
#9909 = LINE ( 'NONE', #12856, #15797 ) ;
#9910 = PRESENTATION_STYLE_ASSIGNMENT (( #5423 ) ) ;
#9911 = CARTESIAN_POINT ( 'NONE',  ( -17.64274437364855430, -28.24771351637087236, 7.326177507916957765 ) ) ;
#9912 = DIRECTION ( 'NONE',  ( -2.775557561562890858E-16, 0.7071067811865454633, 0.7071067811865496822 ) ) ;
#9913 = ORIENTED_EDGE ( 'NONE', *, *, #760, .T. ) ;
#9914 = CARTESIAN_POINT ( 'NONE',  ( -9.955834737091912245, -22.82508104294696594, 36.85742750791696665 ) ) ;
#9915 = CARTESIAN_POINT ( 'NONE',  ( -1.461580736456473462, 62.53841926354353120, 48.05000000109247082 ) ) ;
#9916 = CARTESIAN_POINT ( 'NONE',  ( -18.53959229564982536, -27.78091578003890660, 30.51757249208304401 ) ) ;
#9917 = LINE ( 'NONE', #11484, #14402 ) ;
#9918 = FACE_BOUND ( 'NONE', #13490, .T. ) ;
#9919 = CARTESIAN_POINT ( 'NONE',  ( -15.16482700510259640, -28.99999999999998224, 33.13867750791696665 ) ) ;
#9920 = DIRECTION ( 'NONE',  ( 0.000000000000000000, 0.000000000000000000, -1.000000000000000000 ) ) ;
#9921 = CARTESIAN_POINT ( 'NONE',  ( -17.64274437364855430, -28.24771351637087236, 33.57617750791696665 ) ) ;
#9922 = CARTESIAN_POINT ( 'NONE',  ( -2.500000000000001776, 64.00000000000000000, 46.90000000218494591 ) ) ;
#9923 = CARTESIAN_POINT ( 'NONE',  ( -16.50457296725825174, -19.04416526290807354, 42.76757249208303335 ) ) ;
#9924 = CARTESIAN_POINT ( 'NONE',  ( 1.035533905932739751, 61.50000000000000000, 48.64999999999999858 ) ) ;
#9925 = CARTESIAN_POINT ( 'NONE',  ( -0.8561741729129466183, 61.93301270000000613, 49.10000000109246088 ) ) ;
#9926 = DIRECTION ( 'NONE',  ( -0.000000000000000000, -0.000000000000000000, -1.000000000000000000 ) ) ;
#9927 = CARTESIAN_POINT ( 'NONE',  ( -2.500000000000000888, 62.96446609406726935, 49.24999999999999289 ) ) ;
#9928 = EDGE_CURVE ( 'NONE', #16082, #18276, #70, .T. ) ;
#9929 = CARTESIAN_POINT ( 'NONE',  ( -40.00000000000000711, 110.0000000000000000, 30.00000000000000000 ) ) ;
#9930 = ORIENTED_EDGE ( 'NONE', *, *, #18539, .T. ) ;
#9931 = EDGE_CURVE ( 'NONE', #6170, #9506, #15162, .T. ) ;
#9932 = CARTESIAN_POINT ( 'NONE',  ( 1.461580736456473684, 65.46158073645646880, 46.85000000109246798 ) ) ;
#9933 = CARTESIAN_POINT ( 'NONE',  ( -14.36097942780923731, -27.04416526290806999, 38.16992750791696665 ) ) ;
#9934 = CARTESIAN_POINT ( 'NONE',  ( -41.00000000000000711, 53.00000000000000711, -11.50000000000000000 ) ) ;
#9935 = EDGE_CURVE ( 'NONE', #7747, #2559, #1341, .T. ) ;
#9936 = CARTESIAN_POINT ( 'NONE',  ( -9.996306089212408708, -18.75498260482328661, 27.89257249208303691 ) ) ;
#9937 = CARTESIAN_POINT ( 'NONE',  ( -1.461580736456473462, 62.53841926354353120, 48.25000000109246656 ) ) ;
#9938 = VERTEX_POINT ( 'NONE', #7312 ) ;
#9939 = DIRECTION ( 'NONE',  ( 0.000000000000000000, -1.000000000000000000, 1.471414886128461471E-15 ) ) ;
#9940 = CARTESIAN_POINT ( 'NONE',  ( 2.500000000000002220, 62.96446609406726225, 45.65000000218494591 ) ) ;
#9941 = CARTESIAN_POINT ( 'NONE',  ( 3.796994071234847710E-16, 61.93301269999999903, 46.55000000109247082 ) ) ;
#9942 = CARTESIAN_POINT ( 'NONE',  ( 0.000000000000000000, -0.7390083445627225744, -1.279999999999999138 ) ) ;
#9943 = CIRCLE ( 'NONE', #1522, 0.2000000000000000944 ) ;
#9944 = CARTESIAN_POINT ( 'NONE',  ( -2.500000000000001776, 65.03553390593273775, 49.25000000218494023 ) ) ;
#9945 = CARTESIAN_POINT ( 'NONE',  ( -2.500000000000001776, 64.00000000000000000, 49.65000000109247225 ) ) ;
#9946 = EDGE_CURVE ( 'NONE', #3632, #15274, #10244, .T. ) ;
#9947 = DIRECTION ( 'NONE',  ( -1.000000000000000000, 0.000000000000000000, 0.000000000000000000 ) ) ;
#9948 = ORIENTED_EDGE ( 'NONE', *, *, #13297, .T. ) ;
#9949 = ORIENTED_EDGE ( 'NONE', *, *, #6035, .F. ) ;
#9950 = CARTESIAN_POINT ( 'NONE',  ( -7.955834737091903364, -25.71081734191518464, 2.517572492083039126 ) ) ;
#9951 = SURFACE_STYLE_FILL_AREA ( #1048 ) ;
#9952 = ORIENTED_EDGE ( 'NONE', *, *, #1210, .F. ) ;
#9954 = ORIENTED_EDGE ( 'NONE', *, *, #15603, .F. ) ;
#9953 = VERTEX_POINT ( 'NONE', #2997 ) ;
#9955 = CARTESIAN_POINT ( 'NONE',  ( -16.64274437364856496, -26.51566270880199738, 7.326177507916959541 ) ) ;
#9956 = CARTESIAN_POINT ( 'NONE',  ( -20.24501739517664234, -29.00369391078761439, 28.54492750791695954 ) ) ;
#9957 = AXIS2_PLACEMENT_3D ( 'NONE', #8751, #11788, #1614 ) ;
#9958 = DIRECTION ( 'NONE',  ( -0.7071067811865463515, 0.5000000000000023315, -0.4999999999999994449 ) ) ;
#9959 = CARTESIAN_POINT ( 'NONE',  ( 1.767766952966370653, 62.23223304703363112, 47.20000000218494307 ) ) ;
#9960 = CARTESIAN_POINT ( 'NONE',  ( 0.000000000000000000, 47.00000000000000711, 30.00000000000000000 ) ) ;
#9961 = ORIENTED_EDGE ( 'NONE', *, *, #7576, .F. ) ;
#9962 = LINE ( 'NONE', #15965, #5349 ) ;
#9963 = ORIENTED_EDGE ( 'NONE', *, *, #11373, .T. ) ;
#9964 = ADVANCED_FACE ( 'NONE', ( #13279 ), #19376, .F. ) ;
#9965 = ADVANCED_FACE ( 'NONE', ( #5750 ), #10438, .F. ) ;
#9966 = LINE ( 'NONE', #11250, #16275 ) ;
#9967 = VERTEX_POINT ( 'NONE', #7412 ) ;
#9968 =( NAMED_UNIT ( * ) SI_UNIT ( $, .STERADIAN. ) SOLID_ANGLE_UNIT ( ) );
#9969 = DIRECTION ( 'NONE',  ( 1.000000000000000000, 0.000000000000000000, 2.973811673103096679E-16 ) ) ;
#9970 = DIRECTION ( 'NONE',  ( 1.000000000000000000, 0.000000000000000000, -0.000000000000000000 ) ) ;
#9971 = ADVANCED_FACE ( 'NONE', ( #4678 ), #7217, .T. ) ;
#9972 = CIRCLE ( 'NONE', #9354, 2.500000000000002220 ) ;
#9973 = CARTESIAN_POINT ( 'NONE',  ( 1.461580736456473906, 62.53841926354353120, 46.65000000109247225 ) ) ;
#9974 = DIRECTION ( 'NONE',  ( -1.000000000000000000, -0.000000000000000000, -0.000000000000000000 ) ) ;
#9975 = AXIS2_PLACEMENT_3D ( 'NONE', #1163, #16160, #2826 ) ;
#9976 = CARTESIAN_POINT ( 'NONE',  ( 2.314278491784644842, 64.59068907927618852, 45.00000000000002842 ) ) ;
#9977 = VERTEX_POINT ( 'NONE', #13189 ) ;
#9978 = ORIENTED_EDGE ( 'NONE', *, *, #13207, .T. ) ;
#9979 = CARTESIAN_POINT ( 'NONE',  ( -8.044165262908075320, -26.04047135212042718, 0.5449275079169564329 ) ) ;
#9980 = DIRECTION ( 'NONE',  ( 1.000000000000000000, 0.000000000000000000, 0.000000000000000000 ) ) ;
#9981 = EDGE_LOOP ( 'NONE', ( #7286, #271, #7846, #9242 ) ) ;
#9982 = CARTESIAN_POINT ( 'NONE',  ( -17.07549068051208963, -26.31681416490115311, 9.517572492083044011 ) ) ;
#9983 = CARTESIAN_POINT ( 'NONE',  ( 2.315774708385941683, 31.32836399182263065, 54.80336399182266405 ) ) ;
#9984 = EDGE_CURVE ( 'NONE', #18276, #11674, #5850, .T. ) ;
#9985 = ADVANCED_FACE ( 'NONE', ( #13579 ), #2803, .F. ) ;
#9986 = ORIENTED_EDGE ( 'NONE', *, *, #13231, .F. ) ;
#9987 = CARTESIAN_POINT ( 'NONE',  ( -17.07549068051210739, -21.68318583509881847, 8.857427507916959541 ) ) ;
#9988 = AXIS2_PLACEMENT_3D ( 'NONE', #15322, #1901, #2371 ) ;
#9989 = LINE ( 'NONE', #16081, #1287 ) ;
#9990 = ORIENTED_EDGE ( 'NONE', *, *, #1295, .F. ) ;
#9991 = VECTOR ( 'NONE', #11329, 1000.000000000000000 ) ;
#9992 = DIRECTION ( 'NONE',  ( 0.000000000000000000, -1.000000000000000000, -0.000000000000000000 ) ) ;
#9993 = VERTEX_POINT ( 'NONE', #16432 ) ;
#9994 = DIRECTION ( 'NONE',  ( 0.000000000000000000, -1.000000000000000000, 0.000000000000000000 ) ) ;
#9995 = LINE ( 'NONE', #4031, #11723 ) ;
#9996 = SHAPE_REPRESENTATION ( 'pcba', ( #1791 ), #3902 ) ;
#9997 = LINE ( 'NONE', #16087, #16635 ) ;
#9998 = AXIS2_PLACEMENT_3D ( 'NONE', #17431, #10062, #11345 ) ;
#9999 = LINE ( 'NONE', #3681, #16966 ) ;
#10000 = CARTESIAN_POINT ( 'NONE',  ( -20.04416526290808065, -25.17491895705300209, 28.98242750791695244 ) ) ;
#10001 = AXIS2_PLACEMENT_3D ( 'NONE', #8301, #5550, #18610 ) ;
#10002 = DIRECTION ( 'NONE',  ( -0.000000000000000000, -0.000000000000000000, -1.000000000000000000 ) ) ;
#10003 = CARTESIAN_POINT ( 'NONE',  ( -19.24771351637089367, -21.35725562635142438, 3.388677507916958653 ) ) ;
#10004 = VECTOR ( 'NONE', #15780, 1000.000000000000000 ) ;
#10005 = FACE_OUTER_BOUND ( 'NONE', #18842, .T. ) ;
#10006 = ORIENTED_EDGE ( 'NONE', *, *, #11409, .F. ) ;
#10007 = CARTESIAN_POINT ( 'NONE',  ( -15.16482700510264436, -16.99999999999997868, 42.98632249208304756 ) ) ;
#10008 = CARTESIAN_POINT ( 'NONE',  ( -8.855408670957631401, -20.64274437364852943, 5.138677507916955989 ) ) ;
#10009 = VECTOR ( 'NONE', #13746, 1000.000000000000000 ) ;
#10010 = EDGE_CURVE ( 'NONE', #1960, #14775, #4484, .T. ) ;
#10011 = CARTESIAN_POINT ( 'NONE',  ( -1.461580736456473906, 65.46158073645646880, 47.05000000109247082 ) ) ;
#10012 = CARTESIAN_POINT ( 'NONE',  ( -19.24771351637086880, -26.64274437364857206, 35.98632249208304046 ) ) ;
#10013 = DIRECTION ( 'NONE',  ( -1.000000000000000000, -0.000000000000000000, -0.000000000000000000 ) ) ;
#10014 = VERTEX_POINT ( 'NONE', #11812 ) ;
#10015 = AXIS2_PLACEMENT_3D ( 'NONE', #4632, #407, #3440 ) ;
#10016 = LINE ( 'NONE', #15820, #12515 ) ;
#10017 = CARTESIAN_POINT ( 'NONE',  ( -10.75228648362910100, -26.64274437364854009, 32.26367750791695954 ) ) ;
#10018 = CARTESIAN_POINT ( 'NONE',  ( 0.1249999999999895917, 33.66708332270461312, 52.46464466094069934 ) ) ;
#10019 = FACE_OUTER_BOUND ( 'NONE', #906, .T. ) ;
#10020 = AXIS2_PLACEMENT_3D ( 'NONE', #11355, #2538, #11540 ) ;
#10021 = CARTESIAN_POINT ( 'NONE',  ( 0.1249999999999895917, 25.64142146683625612, 60.84290755733282197 ) ) ;
#10022 = CARTESIAN_POINT ( 'NONE',  ( -13.49542703274174116, -28.95583473709188738, 40.14257249208304046 ) ) ;
#10023 = CARTESIAN_POINT ( 'NONE',  ( -1.035533905932738863, 61.50000000000000000, 46.95000000000000995 ) ) ;
#10024 = CARTESIAN_POINT ( 'NONE',  ( -2.500000000000003553, 62.96446609406726225, 49.24999999999997868 ) ) ;
#10025 = VECTOR ( 'NONE', #3143, 1000.000000000000000 ) ;
#10026 = CARTESIAN_POINT ( 'NONE',  ( -1.035533905932738863, 61.50000000000000000, 48.65000000218493881 ) ) ;
#10027 = CARTESIAN_POINT ( 'NONE',  ( -2.066987300000001415, 64.00000000000000000, 45.75000000109247367 ) ) ;
#10028 = CARTESIAN_POINT ( 'NONE',  ( -2.500000000000001776, 64.00000000000000000, 48.39999999999999858 ) ) ;
#10029 = VECTOR ( 'NONE', #14238, 1000.000000000000000 ) ;
#10030 = ORIENTED_EDGE ( 'NONE', *, *, #13564, .T. ) ;
#10031 = VECTOR ( 'NONE', #6223, 1000.000000000000000 ) ;
#10032 = SURFACE_STYLE_USAGE ( .BOTH. , #16415 ) ;
#10033 = EDGE_CURVE ( 'NONE', #8432, #13561, #16004, .T. ) ;
#10034 = CARTESIAN_POINT ( 'NONE',  ( -1.265664690411616068E-16, 66.06698730000000808, 44.55000000109247082 ) ) ;
#10035 = ADVANCED_FACE ( 'NONE', ( #10342 ), #17503, .F. ) ;
#10036 = CARTESIAN_POINT ( 'NONE',  ( -10.04416526290807710, -25.50457296725819489, 0.5449275079169579872 ) ) ;
#10037 = FACE_OUTER_BOUND ( 'NONE', #2543, .T. ) ;
#10038 = CARTESIAN_POINT ( 'NONE',  ( -18.64274437364860049, -18.02023567606023491, 37.29882249208304046 ) ) ;
#10039 = VECTOR ( 'NONE', #6262, 1000.000000000000000 ) ;
#10040 = CARTESIAN_POINT ( 'NONE',  ( 0.8561741729129460632, 66.06698729999999387, 48.70000000109247651 ) ) ;
#10041 = CARTESIAN_POINT ( 'NONE',  ( -12.31951028609537602, -22.64274437364854364, 26.13867750791696309 ) ) ;
#10042 = CARTESIAN_POINT ( 'NONE',  ( -19.95583473709191225, -22.49542703274176603, 3.169927507916957765 ) ) ;
#10043 = FACE_OUTER_BOUND ( 'NONE', #12587, .T. ) ;
#10044 = AXIS2_PLACEMENT_3D ( 'NONE', #14661, #17912, #1233 ) ;
#10045 = CARTESIAN_POINT ( 'NONE',  ( 3.796994071234847710E-16, 61.93301269999999903, 45.75000000109247367 ) ) ;
#10046 = CARTESIAN_POINT ( 'NONE',  ( 2.500000000000000000, 0.000000000000000000, 0.000000000000000000 ) ) ;
#10047 = CARTESIAN_POINT ( 'NONE',  ( -44.99999999999998579, -1.285879139104706187E-16, -53.40000000000000568 ) ) ;
#10048 = DIRECTION ( 'NONE',  ( -1.156482317317871478E-16, 1.000000000000000000, 0.000000000000000000 ) ) ;
#10049 = CARTESIAN_POINT ( 'NONE',  ( -40.00000000000000711, 110.0000000000000000, 30.00000000000000000 ) ) ;
#10050 = ORIENTED_EDGE ( 'NONE', *, *, #7396, .F. ) ;
#10051 = VERTEX_POINT ( 'NONE', #437 ) ;
#10052 = CARTESIAN_POINT ( 'NONE',  ( -21.95583473709189803, -26.04047135212049469, 4.705072492083038682 ) ) ;
#10053 = FILL_AREA_STYLE ('',( #8787 ) ) ;
#10054 = VERTEX_POINT ( 'NONE', #16905 ) ;
#10056 = ORIENTED_EDGE ( 'NONE', *, *, #10236, .F. ) ;
#10055 = ORIENTED_EDGE ( 'NONE', *, *, #4571, .F. ) ;
#10057 = CARTESIAN_POINT ( 'NONE',  ( -17.99999999999999645, -24.16482700510260173, 41.67382249208304756 ) ) ;
#10058 = CARTESIAN_POINT ( 'NONE',  ( -9.996306089212364299, -29.24501739517662813, 32.48242750791695244 ) ) ;
#10059 = VECTOR ( 'NONE', #5677, 1000.000000000000000 ) ;
#10060 = LINE ( 'NONE', #2426, #16989 ) ;
#10061 = CARTESIAN_POINT ( 'NONE',  ( 2.066987300000001415, 64.00000000000000000, 48.35000000109246798 ) ) ;
#10062 = DIRECTION ( 'NONE',  ( 0.000000000000000000, 0.7071067811865456854, 0.7071067811865494601 ) ) ;
#10063 = ORIENTED_EDGE ( 'NONE', *, *, #4708, .F. ) ;
#10064 = ADVANCED_FACE ( 'NONE', ( #13757 ), #6615, .F. ) ;
#10065 = LINE ( 'NONE', #18635, #7539 ) ;
#10066 = ORIENTED_EDGE ( 'NONE', *, *, #1423, .F. ) ;
#10067 = LINE ( 'NONE', #9262, #3589 ) ;
#10068 = VERTEX_POINT ( 'NONE', #3375 ) ;
#10069 = CARTESIAN_POINT ( 'NONE',  ( -0.5386384701873604408, 61.99983965256841856, 45.00000000000003553 ) ) ;
#10070 = DIRECTION ( 'NONE',  ( -0.000000000000000000, -0.000000000000000000, -1.000000000000000000 ) ) ;
#10071 = DIRECTION ( 'NONE',  ( 0.7071067811865414665, -0.5000000000000058842, 0.5000000000000028866 ) ) ;
#10072 = CARTESIAN_POINT ( 'NONE',  ( -2.066987300000001859, 64.85617417291294373, 47.10000000109246798 ) ) ;
#10073 = DIRECTION ( 'NONE',  ( -0.000000000000000000, 1.000000000000000000, -0.000000000000000000 ) ) ;
#10074 = CARTESIAN_POINT ( 'NONE',  ( -41.00000000000000711, 110.0000000000000000, -18.00000000000000000 ) ) ;
#10075 = DIRECTION ( 'NONE',  ( -1.000000000000000000, 0.000000000000000000, 0.000000000000000000 ) ) ;
#10076 = ORIENTED_EDGE ( 'NONE', *, *, #7601, .F. ) ;
#10078 = VERTEX_POINT ( 'NONE', #15331 ) ;
#10077 = ORIENTED_EDGE ( 'NONE', *, *, #10732, .T. ) ;
#10079 = CARTESIAN_POINT ( 'NONE',  ( -13.28918265808472299, -31.04416526290805933, 1.419927507916956433 ) ) ;
#10080 = DIRECTION ( 'NONE',  ( 1.000000000000000000, -0.000000000000000000, -0.000000000000000000 ) ) ;
#10081 = ORIENTED_EDGE ( 'NONE', *, *, #17357, .T. ) ;
#10082 = EDGE_CURVE ( 'NONE', #7137, #7631, #14050, .T. ) ;
#10083 = CARTESIAN_POINT ( 'NONE',  ( -10.58745947852648328, -26.35725562635138530, 39.48632249208304046 ) ) ;
#10084 = EDGE_CURVE ( 'NONE', #16683, #9604, #15437, .T. ) ;
#10085 = CARTESIAN_POINT ( 'NONE',  ( -3.999999999999996447, 47.00000000000000711, 34.99999999999999289 ) ) ;
#10086 = EDGE_LOOP ( 'NONE', ( #17755, #15728, #12130, #3980, #12907, #12436, #10867, #9860, #11936, #4717, #6079, #13523, #10958, #16484, #750, #18311, #6246, #18350, #5491, #17226, #18677, #12449, #13639, #7942, #11845, #10875, #1169, #12719, #2279, #14807, #7756, #13595 ) ) ;
#10087 = CARTESIAN_POINT ( 'NONE',  ( -18.04416526290808420, -24.63902057219074493, 2.732427507916960430 ) ) ;
#10088 = CARTESIAN_POINT ( 'NONE',  ( -2.500000000000001776, 64.00000000000000000, 47.59999999999999432 ) ) ;
#10089 = VERTEX_POINT ( 'NONE', #6324 ) ;
#10090 = CARTESIAN_POINT ( 'NONE',  ( -40.00000000000000000, 53.00000000000000711, 30.00000000000000000 ) ) ;
#10091 = VERTEX_POINT ( 'NONE', #13956 ) ;
#10092 = CARTESIAN_POINT ( 'NONE',  ( -3.155775640247338920, -41.39960408384398249, 1.500000000000000000 ) ) ;
#10093 = DIRECTION ( 'NONE',  ( 1.000000000000000000, 0.000000000000000000, 0.000000000000000000 ) ) ;
#10094 = CARTESIAN_POINT ( 'NONE',  ( -41.00000000000000711, 110.0000000000000000, 0.5000000000000004441 ) ) ;
#10095 =( NAMED_UNIT ( * ) SI_UNIT ( $, .STERADIAN. ) SOLID_ANGLE_UNIT ( ) );
#10096 = CARTESIAN_POINT ( 'NONE',  ( -2.500000000000001776, 64.00000000000000000, 49.99999999999999289 ) ) ;
#10097 = CARTESIAN_POINT ( 'NONE',  ( -19.41254052147348830, -26.35725562635142083, 23.51367750791695954 ) ) ;
#10098 = FACE_BOUND ( 'NONE', #7345, .T. ) ;
#10099 = CARTESIAN_POINT ( 'NONE',  ( -11.46040770435012668, -27.78091578003887463, 6.232427507916956877 ) ) ;
#10100 = DIRECTION ( 'NONE',  ( 0.000000000000000000, 0.7071067811865454633, 0.7071067811865496822 ) ) ;
#10101 = EDGE_CURVE ( 'NONE', #8595, #6698, #9157, .T. ) ;
#10102 = EDGE_LOOP ( 'NONE', ( #8603, #17081, #9656, #7028 ) ) ;
#10103 = CARTESIAN_POINT ( 'NONE',  ( -19.41254052147350961, -21.64274437364857562, 10.61132249208304046 ) ) ;
#10104 = CARTESIAN_POINT ( 'NONE',  ( -12.95952864787955150, -17.04416526290805933, 4.482427507916956877 ) ) ;
#10105 = CARTESIAN_POINT ( 'NONE',  ( 0.8561741729129472844, 61.93301270000000613, 46.60000000109246088 ) ) ;
#10106 = EDGE_CURVE ( 'NONE', #11279, #11949, #17009, .T. ) ;
#10107 = CARTESIAN_POINT ( 'NONE',  ( -11.95583473709190514, -24.63902057219072361, 7.767572492083043123 ) ) ;
#10108 = LINE ( 'NONE', #12956, #2505 ) ;
#10109 = ORIENTED_EDGE ( 'NONE', *, *, #4837, .F. ) ;
#10110 = LINE ( 'NONE', #9826, #1881 ) ;
#10111 = CARTESIAN_POINT ( 'NONE',  ( -9.955834737091912245, -22.82508104294696594, 36.85742750791696665 ) ) ;
#10112 = PLANE ( 'NONE',  #5471 ) ;
#10113 = CARTESIAN_POINT ( 'NONE',  ( 1.035533905932738197, 66.50000000000000000, 45.05000000218493739 ) ) ;
#10114 = DIRECTION ( 'NONE',  ( 0.000000000000000000, 0.000000000000000000, 1.000000000000000000 ) ) ;
#10115 = CARTESIAN_POINT ( 'NONE',  ( -10.04416526290808598, -22.49542703274172695, 33.58007249208303335 ) ) ;
#10116 = CARTESIAN_POINT ( 'NONE',  ( -2.500000000000000888, 62.96446609406726935, 47.64999999999999858 ) ) ;
#10117 = CARTESIAN_POINT ( 'NONE',  ( -1.461580736456473906, 65.46158073645646880, 49.65000000109246514 ) ) ;
#10118 = EDGE_CURVE ( 'NONE', #13021, #7331, #18288, .T. ) ;
#10119 = DIRECTION ( 'NONE',  ( -0.000000000000000000, -1.000000000000000000, -0.000000000000000000 ) ) ;
#10120 = CARTESIAN_POINT ( 'NONE',  ( -1.035533905932738863, 61.50000000000000000, 45.34999999999999432 ) ) ;
#10121 = DIRECTION ( 'NONE',  ( 0.000000000000000000, -1.000000000000000000, 0.000000000000000000 ) ) ;
#10122 = ORIENTED_EDGE ( 'NONE', *, *, #5557, .T. ) ;
#10123 = DIRECTION ( 'NONE',  ( 0.000000000000000000, 0.000000000000000000, 1.000000000000000000 ) ) ;
#10124 = DIRECTION ( 'NONE',  ( -0.5773502691896202910, 0.8164965809277299202, 0.000000000000000000 ) ) ;
#10125 = PRESENTATION_LAYER_ASSIGNMENT (  '', '', ( #4520 ) ) ;
#10126 = CARTESIAN_POINT ( 'NONE',  ( -12.92450931948788906, -26.31681416490114245, 37.73242750791696665 ) ) ;
#10127 = CARTESIAN_POINT ( 'NONE',  ( -1.530808498934192803E-16, 66.50000000000000000, 48.99999999999999289 ) ) ;
#10128 = CARTESIAN_POINT ( 'NONE',  ( -20.04416526290809131, -22.82508104294699791, 5.142572492083038682 ) ) ;
#10129 = MANIFOLD_SOLID_BREP ( 'CirPattern1', #88 ) ;
#10130 = CARTESIAN_POINT ( 'NONE',  ( -1.265664690411616068E-16, 66.06698730000000808, 47.15000000109247225 ) ) ;
#10131 = CARTESIAN_POINT ( 'NONE',  ( -18.04416526290808420, -24.63902057219074493, 34.23242750791695954 ) ) ;
#10132 = DIRECTION ( 'NONE',  ( 1.000000000000000000, -0.000000000000000000, -0.000000000000000000 ) ) ;
#10133 = LINE ( 'NONE', #12982, #9121 ) ;
#10134 = LINE ( 'NONE', #1231, #15318 ) ;
#10135 = CARTESIAN_POINT ( 'NONE',  ( -3.155775640247338920, -38.39960408384397539, 1.500000000000000000 ) ) ;
#10136 = CARTESIAN_POINT ( 'NONE',  ( -11.75000000000000000, -35.50000000000000000, 5.500000000000000000 ) ) ;
#10137 = AXIS2_PLACEMENT_3D ( 'NONE', #19253, #12182, #18181 ) ;
#10138 = CARTESIAN_POINT ( 'NONE',  ( -0.8561741729129461742, 66.06698730000000808, 48.80000000109247082 ) ) ;
#10139 = CARTESIAN_POINT ( 'NONE',  ( 2.500000000000001776, 64.00000000000000000, 48.79999999999999716 ) ) ;
#10140 = CARTESIAN_POINT ( 'NONE',  ( 4.592425496802577917E-16, 61.50000000000000000, 44.70000000218494307 ) ) ;
#10141 = ORIENTED_EDGE ( 'NONE', *, *, #10118, .F. ) ;
#10142 = ORIENTED_EDGE ( 'NONE', *, *, #16772, .T. ) ;
#10143 = CARTESIAN_POINT ( 'NONE',  ( -17.04047135212043784, -30.95583473709190159, 38.60742750791695954 ) ) ;
#10144 = ORIENTED_EDGE ( 'NONE', *, *, #9414, .F. ) ;
#10146 = ORIENTED_EDGE ( 'NONE', *, *, #19335, .F. ) ;
#10145 = ORIENTED_EDGE ( 'NONE', *, *, #8174, .T. ) ;
#10147 = CARTESIAN_POINT ( 'NONE',  ( -18.04416526290808420, -24.63902057219074493, 2.732427507916960430 ) ) ;
#10148 = CARTESIAN_POINT ( 'NONE',  ( -14.83517299489740715, -16.99999999999997868, 30.51367750791695954 ) ) ;
#10149 = PRODUCT_DEFINITION_FORMATION_WITH_SPECIFIED_SOURCE ( 'ANY', '', #18808, .NOT_KNOWN. ) ;
#10150 = AXIS2_PLACEMENT_3D ( 'NONE', #16879, #2072, #10779 ) ;
#10151 = CARTESIAN_POINT ( 'NONE',  ( 1.300000000000000044, 1.478016689125442484, -1.626303258728256651E-15 ) ) ;
#10152 = CARTESIAN_POINT ( 'NONE',  ( -2.500000000000000888, 62.96446609406726935, 45.35000000218493454 ) ) ;
#10153 = CARTESIAN_POINT ( 'NONE',  ( -41.00000000000000711, 110.0000000000000000, -37.50000000000000711 ) ) ;
#10154 = ORIENTED_EDGE ( 'NONE', *, *, #10715, .F. ) ;
#10155 = DIRECTION ( 'NONE',  ( 0.000000000000000000, 0.000000000000000000, -1.000000000000000000 ) ) ;
#10156 = ORIENTED_EDGE ( 'NONE', *, *, #1505, .F. ) ;
#10157 = VERTEX_POINT ( 'NONE', #1807 ) ;
#10158 = DIRECTION ( 'NONE',  ( -0.000000000000000000, -0.000000000000000000, -1.000000000000000000 ) ) ;
#10159 = FACE_OUTER_BOUND ( 'NONE', #5105, .T. ) ;
#10160 = CARTESIAN_POINT ( 'NONE',  ( -2.500000000000001776, 64.00000000000000000, 49.99999999999999289 ) ) ;
#10161 = CARTESIAN_POINT ( 'NONE',  ( -2.066987300000001859, 64.85617417291294373, 49.70000000109248361 ) ) ;
#10162 = CARTESIAN_POINT ( 'NONE',  ( -24.00000000000000000, 53.00000000000000711, -24.49999999999999289 ) ) ;
#10163 = AXIS2_PLACEMENT_3D ( 'NONE', #19309, #5978, #4212 ) ;
#10164 = FACE_OUTER_BOUND ( 'NONE', #17147, .T. ) ;
#10165 = VECTOR ( 'NONE', #15926, 1000.000000000000000 ) ;
#10166 = CARTESIAN_POINT ( 'NONE',  ( 44.99999999999997158, 3.000000000000000000, 55.00000000000000000 ) ) ;
#10167 = ORIENTED_EDGE ( 'NONE', *, *, #6725, .T. ) ;
#10169 = ORIENTED_EDGE ( 'NONE', *, *, #17800, .T. ) ;
#10168 = ORIENTED_EDGE ( 'NONE', *, *, #15836, .F. ) ;
#10170 = ADVANCED_FACE ( 'NONE', ( #7895, #7789 ), #18386, .T. ) ;
#10172 = ADVANCED_FACE ( 'NONE', ( #12478 ), #10612, .F. ) ;
#10171 = CARTESIAN_POINT ( 'NONE',  ( -9.996306089212364299, -29.24501739517662813, 6.232427507916955989 ) ) ;
#10173 = CARTESIAN_POINT ( 'NONE',  ( -15.16482700510263371, -18.99999999999997868, 0.9863224920830410136 ) ) ;
#10174 = ORIENTED_EDGE ( 'NONE', *, *, #6964, .T. ) ;
#10175 = VERTEX_POINT ( 'NONE', #15141 ) ;
#10176 = CARTESIAN_POINT ( 'NONE',  ( -17.35725562635140307, -28.41254052147349185, 40.79882249208304046 ) ) ;
#10177 = ADVANCED_FACE ( 'NONE', ( #1708 ), #7689, .F. ) ;
#10178 = DIRECTION ( 'NONE',  ( -1.888166612144349831E-32, 1.000000000000000000, 1.632680918566406793E-16 ) ) ;
#10179 = ORIENTED_EDGE ( 'NONE', *, *, #756, .T. ) ;
#10180 = CARTESIAN_POINT ( 'NONE',  ( -17.07549068051208963, -26.31681416490115311, 41.01757249208304756 ) ) ;
#10181 = EDGE_CURVE ( 'NONE', #1809, #18891, #12947, .T. ) ;
#10182 = AXIS2_PLACEMENT_3D ( 'NONE', #19085, #8880, #10245 ) ;
#10183 = LINE ( 'NONE', #19324, #8475 ) ;
#10184 = VERTEX_POINT ( 'NONE', #15903 ) ;
#10185 = AXIS2_PLACEMENT_3D ( 'NONE', #3181, #341, #16615 ) ;
#10186 = DIRECTION ( 'NONE',  ( 0.000000000000000000, -0.000000000000000000, -1.000000000000000000 ) ) ;
#10187 = PRODUCT ( 'pcba', 'pcba', '', ( #10290 ) ) ;
#10188 = EDGE_LOOP ( 'NONE', ( #18902, #5768, #5292, #11263, #7146 ) ) ;
#10189 = LINE ( 'NONE', #5896, #14734 ) ;
#10190 = DIRECTION ( 'NONE',  ( 3.826732013112563602E-16, -1.000000000000000000, 0.000000000000000000 ) ) ;
#10191 = LINE ( 'NONE', #7070, #6314 ) ;
#10192 = PRODUCT_CONTEXT ( 'NONE', #3690, 'mechanical' ) ;
#10193 = CARTESIAN_POINT ( 'NONE',  ( -24.00000000000000000, 0.000000000000000000, -67.72004514666936359 ) ) ;
#10194 = ADVANCED_FACE ( 'NONE', ( #15724 ), #3852, .T. ) ;
#10195 = CARTESIAN_POINT ( 'NONE',  ( -11.21908421996108629, -20.46040770435011069, 25.91992750791694888 ) ) ;
#10196 = FACE_OUTER_BOUND ( 'NONE', #19312, .T. ) ;
#10197 = CARTESIAN_POINT ( 'NONE',  ( -14.83517299489739649, -18.99999999999997868, -0.9863224920830417908 ) ) ;
#10198 = MANIFOLD_SOLID_BREP ( 'Chamfer1', #14175 ) ;
#10199 = AXIS2_PLACEMENT_3D ( 'NONE', #1691, #7277, #5805 ) ;
#10200 = DIRECTION ( 'NONE',  ( 1.000000000000000000, 0.000000000000000000, 0.000000000000000000 ) ) ;
#10201 = ORIENTED_EDGE ( 'NONE', *, *, #14752, .F. ) ;
#10202 = VECTOR ( 'NONE', #4639, 1000.000000000000000 ) ;
#10203 = EDGE_CURVE ( 'NONE', #19297, #16534, #9134, .T. ) ;
#10204 = CARTESIAN_POINT ( 'NONE',  ( -19.24771351637086880, -26.64274437364857206, 4.486322492083041347 ) ) ;
#10205 = CARTESIAN_POINT ( 'NONE',  ( -21.14459132904236327, -27.35725562635143149, 7.763677507916957765 ) ) ;
#10206 = CARTESIAN_POINT ( 'NONE',  ( 2.066987300000002303, 63.14382582708705627, 45.90000000109247225 ) ) ;
#10207 = CARTESIAN_POINT ( 'NONE',  ( -18.78091578003892081, -20.46040770435013556, 42.33007249208301914 ) ) ;
#10208 = CARTESIAN_POINT ( 'NONE',  ( -1.767766952966369765, 62.23223304703363112, 48.49999999999999289 ) ) ;
#10209 = ORIENTED_EDGE ( 'NONE', *, *, #7869, .T. ) ;
#10210 = CARTESIAN_POINT ( 'NONE',  ( 0.000000000000000000, -2.357898499370432610, 3.252606517456513302E-15 ) ) ;
#10211 = CARTESIAN_POINT ( 'NONE',  ( -20.04416526290808065, -25.17491895705300209, 39.48242750791695244 ) ) ;
#10212 = CARTESIAN_POINT ( 'NONE',  ( 0.000000000000000000, 3.000000000000000000, 51.99999999999997868 ) ) ;
#10213 = CIRCLE ( 'NONE', #11786, 1.600000000000000311 ) ;
#10214 = DIRECTION ( 'NONE',  ( -1.000000000000000000, -0.000000000000000000, -0.000000000000000000 ) ) ;
#10215 = FACE_BOUND ( 'NONE', #19289, .T. ) ;
#10216 = CARTESIAN_POINT ( 'NONE',  ( -9.955834737091903364, -25.17491895705295235, 34.01757249208303335 ) ) ;
#10217 = ADVANCED_FACE ( 'NONE', ( #18944 ), #15619, .T. ) ;
#10218 = CIRCLE ( 'NONE', #8660, 1.500000000000001332 ) ;
#10219 = EDGE_CURVE ( 'NONE', #18580, #15589, #9815, .T. ) ;
#10220 = CARTESIAN_POINT ( 'NONE',  ( -1.767766952966369765, 62.23223304703363112, 46.09999999999999432 ) ) ;
#10221 = CARTESIAN_POINT ( 'NONE',  ( -2.066987300000001415, 64.00000000000000000, 45.75000000109247367 ) ) ;
#10222 = ADVANCED_FACE ( 'NONE', ( #18858 ), #18577, .F. ) ;
#10223 = LINE ( 'NONE', #10318, #4203 ) ;
#10224 = ADVANCED_FACE ( 'NONE', ( #3945 ), #3665, .F. ) ;
#10225 = CARTESIAN_POINT ( 'NONE',  ( 1.035533905932738197, 66.50000000000000000, 48.14999999999999858 ) ) ;
#10226 = LINE ( 'NONE', #2589, #4589 ) ;
#10227 = ORIENTED_EDGE ( 'NONE', *, *, #19263, .T. ) ;
#10228 = B_SPLINE_CURVE_WITH_KNOTS ( 'NONE', 3,
 ( #19011, #3723, #11443, #6850, #5576, #10069, #14214, #12822, #17437, #14591, #3823, #9789, #15970, #2348 ),
 .UNSPECIFIED., .F., .F.,
 ( 4, 2, 2, 2, 2, 2, 4 ),
 ( 1.446806763283639067E-16, 0.0008152643689841970439, 0.001222896553476223412, 0.001630528737968249889, 0.002038160922460276366, 0.002445793106952302842, 0.003261057475936356663 ),
 .UNSPECIFIED. ) ;
#10229 = PRESENTATION_LAYER_ASSIGNMENT (  '', '', ( #7753 ) ) ;
#10230 =( BOUNDED_CURVE ( )  B_SPLINE_CURVE ( 2, ( #19048, #5430, #5086, #5722, #14533, #4047, #10208, #11388, #7085 ),
 .UNSPECIFIED., .F., .F. ) 
 B_SPLINE_CURVE_WITH_KNOTS ( ( 3, 2, 2, 2, 3 ),
 ( 0.2142857142857141350, 0.2321428571428569565, 0.2499999999999997224, 0.2678571428571425161, 0.2857142857142853098 ),
 .UNSPECIFIED. ) 
 CURVE ( )  GEOMETRIC_REPRESENTATION_ITEM ( )  RATIONAL_B_SPLINE_CURVE ( ( 1.000000000000000666, 0.9238795325112861834, 1.000000000000000000, 0.9238795325112867385, 1.000000000000000000, 0.9238795325112867385, 1.000000000000000000, 0.9238795325112884038, 0.9999999999999983347 ) ) 
 REPRESENTATION_ITEM ( '' )  );
#10231 = CARTESIAN_POINT ( 'NONE',  ( -18.78091578003889950, -27.53959229564985378, 2.294927507916958209 ) ) ;
#10232 = CARTESIAN_POINT ( 'NONE',  ( -14.83517299489738761, -20.99999999999997513, 41.01367750791695954 ) ) ;
#10233 = CARTESIAN_POINT ( 'NONE',  ( -25.00000000000000711, -6.000000000000000000, -42.50000000000001421 ) ) ;
#10234 = CARTESIAN_POINT ( 'NONE',  ( -13.82508104294702100, -18.95583473709188382, 1.205072492083041125 ) ) ;
#10235 = CARTESIAN_POINT ( 'NONE',  ( -2.066987300000001415, 64.00000000000000000, 47.35000000109246798 ) ) ;
#10236 = EDGE_CURVE ( 'NONE', #2028, #8784, #722, .T. ) ;
#10237 = CARTESIAN_POINT ( 'NONE',  ( -14.83517299489739649, -18.99999999999997868, -0.9863224920830417908 ) ) ;
#10238 = CARTESIAN_POINT ( 'NONE',  ( -9.999999999999994671, -24.16482700510257686, 0.3261775079169582647 ) ) ;
#10239 = CARTESIAN_POINT ( 'NONE',  ( 2.500000000000000000, -2.629050547790028551E-15, -2.041999999999999815 ) ) ;
#10240 = LINE ( 'NONE', #16133, #13422 ) ;
#10241 = CYLINDRICAL_SURFACE ( 'NONE', #3713, 1.500000000000001332 ) ;
#10242 = CARTESIAN_POINT ( 'NONE',  ( 0.000000000000000000, 64.00000000000000000, 49.99999999999999289 ) ) ;
#10243 = CARTESIAN_POINT ( 'NONE',  ( 2.066987300000001859, 63.14382582708704916, 49.30000000109246372 ) ) ;
#10244 = LINE ( 'NONE', #4284, #13488 ) ;
#10245 = DIRECTION ( 'NONE',  ( -1.000000000000000000, 0.000000000000000000, -0.000000000000000000 ) ) ;
#10246 = ORIENTED_EDGE ( 'NONE', *, *, #13664, .F. ) ;
#10247 = ORIENTED_EDGE ( 'NONE', *, *, #2934, .T. ) ;
#10248 = CARTESIAN_POINT ( 'NONE',  ( -9.996306089212408708, -18.75498260482328661, 22.64257249208304046 ) ) ;
#10249 = CARTESIAN_POINT ( 'NONE',  ( -17.35725562635140307, -28.41254052147349185, 4.048822492083041347 ) ) ;
#10251 = VERTEX_POINT ( 'NONE', #18672 ) ;
#10250 = ORIENTED_EDGE ( 'NONE', *, *, #5789, .T. ) ;
#10252 = CARTESIAN_POINT ( 'NONE',  ( -13.35725562635142794, -21.48433729119796709, 4.701177507916959541 ) ) ;
#10253 = CARTESIAN_POINT ( 'NONE',  ( -12.95952864787948755, -30.95583473709188382, 3.392572492083039570 ) ) ;
#10254 = LINE ( 'NONE', #1354, #2869 ) ;
#10255 = CARTESIAN_POINT ( 'NONE',  ( 1.035533905932739751, 61.50000000000000000, 44.75000000218494023 ) ) ;
#10256 = ORIENTED_EDGE ( 'NONE', *, *, #5541, .T. ) ;
#10257 = EDGE_CURVE ( 'NONE', #15240, #17638, #9728, .T. ) ;
#10258 = EDGE_LOOP ( 'NONE', ( #15480, #13709, #14792 ) ) ;
#10259 = DIRECTION ( 'NONE',  ( 0.000000000000000000, 1.000000000000000000, -0.000000000000000000 ) ) ;
#10260 = ORIENTED_EDGE ( 'NONE', *, *, #12811, .T. ) ;
#10261 = ORIENTED_EDGE ( 'NONE', *, *, #3875, .F. ) ;
#10262 = DIRECTION ( 'NONE',  ( 0.000000000000000000, -0.000000000000000000, -1.000000000000000000 ) ) ;
#10263 = CARTESIAN_POINT ( 'NONE',  ( -1.040834085586084257E-14, 25.49999999999996803, 52.49999999999998579 ) ) ;
#10264 = DIRECTION ( 'NONE',  ( 0.000000000000000000, 0.000000000000000000, 1.000000000000000000 ) ) ;
#10265 = CARTESIAN_POINT ( 'NONE',  ( -2.066987300000001859, 64.85617417291294373, 47.30000000109247082 ) ) ;
#10266 = LINE ( 'NONE', #2929, #19108 ) ;
#10267 = DIRECTION ( 'NONE',  ( -0.000000000000000000, -1.000000000000000000, -0.000000000000000000 ) ) ;
#10268 = VERTEX_POINT ( 'NONE', #15592 ) ;
#10270 = VERTEX_POINT ( 'NONE', #9411 ) ;
#10269 = ORIENTED_EDGE ( 'NONE', *, *, #13095, .F. ) ;
#10271 = CARTESIAN_POINT ( 'NONE',  ( -13.28918265808472299, -31.04416526290805933, 6.669927507916955989 ) ) ;
#10272 = VECTOR ( 'NONE', #17303, 1000.000000000000000 ) ;
#10273 = CARTESIAN_POINT ( 'NONE',  ( -2.500000000000006661, 65.03553390593272354, 45.14999999999999858 ) ) ;
#10274 = ORIENTED_EDGE ( 'NONE', *, *, #2574, .F. ) ;
#10275 = ORIENTED_EDGE ( 'NONE', *, *, #4708, .T. ) ;
#10276 = CARTESIAN_POINT ( 'NONE',  ( -12.04416526290808420, -23.03132541760398766, 2.080072492083043567 ) ) ;
#10277 = CARTESIAN_POINT ( 'NONE',  ( -41.00000000000000711, 53.00000000000000711, 14.50000000000000000 ) ) ;
#10278 = CARTESIAN_POINT ( 'NONE',  ( -1.767766952966369765, 62.23223304703363112, 47.00000000218494733 ) ) ;
#10279 = EDGE_LOOP ( 'NONE', ( #7181, #3720, #12717, #4840 ) ) ;
#10280 = CARTESIAN_POINT ( 'NONE',  ( -15.96867458239597326, -26.95583473709190159, 1.857427507916959986 ) ) ;
#10281 = CIRCLE ( 'NONE', #3726, 1.249999999999999334 ) ;
#10282 = CARTESIAN_POINT ( 'NONE',  ( -1.767766952966370209, 65.76776695296638309, 44.40000000218493881 ) ) ;
#10283 = ORIENTED_EDGE ( 'NONE', *, *, #2574, .T. ) ;
#10284 = CARTESIAN_POINT ( 'NONE',  ( 0.000000000000000000, 47.00000000000000711, 30.00000000000000000 ) ) ;
#10285 = VERTEX_POINT ( 'NONE', #12551 ) ;
#10286 = LINE ( 'NONE', #4432, #5353 ) ;
#10287 = CARTESIAN_POINT ( 'NONE',  ( 2.039008344562727615, -1.214068345727601445E-18, 0.000000000000000000 ) ) ;
#10288 = VECTOR ( 'NONE', #8855, 1000.000000000000000 ) ;
#10289 = CARTESIAN_POINT ( 'NONE',  ( -24.00000000000000711, 53.00000000000000711, -6.000000000000001776 ) ) ;
#10290 = PRODUCT_CONTEXT ( 'NONE', #5698, 'mechanical' ) ;
#10291 = CARTESIAN_POINT ( 'NONE',  ( -41.00000000000000711, 53.00000000000000711, -30.99999999999999645 ) ) ;
#10292 = CARTESIAN_POINT ( 'NONE',  ( -19.99999999999999645, -23.83517299489738051, 23.95117750791695954 ) ) ;
#10293 = CARTESIAN_POINT ( 'NONE',  ( -2.500000000000001776, 64.00000000000000000, 34.99999999999999289 ) ) ;
#10294 = CARTESIAN_POINT ( 'NONE',  ( -15.16482700510259640, -28.99999999999998224, 6.888677507916957765 ) ) ;
#10295 = AXIS2_PLACEMENT_3D ( 'NONE', #17975, #15034, #4456 ) ;
#10296 = FACE_OUTER_BOUND ( 'NONE', #5676, .T. ) ;
#10297 = VERTEX_POINT ( 'NONE', #18258 ) ;
#10298 = CARTESIAN_POINT ( 'NONE',  ( -12.64274437364858628, -19.58745947852646552, 1.423822492083040903 ) ) ;
#10299 = CIRCLE ( 'NONE', #3111, 1.599999999999997202 ) ;
#10300 = CARTESIAN_POINT ( 'NONE',  ( -18.64274437364853654, -29.97976432393976509, 2.076177507916956433 ) ) ;
#10301 = VECTOR ( 'NONE', #18613, 1000.000000000000000 ) ;
#10302 = DIRECTION ( 'NONE',  ( 0.000000000000000000, 0.000000000000000000, 1.000000000000000000 ) ) ;
#10303 = CARTESIAN_POINT ( 'NONE',  ( -12.68318583509882380, -26.07549068051207541, 2.955072492083043123 ) ) ;
#10304 = CARTESIAN_POINT ( 'NONE',  ( -2.500000000000001776, 64.00000000000000000, 46.00000000000000000 ) ) ;
#10305 = ORIENTED_EDGE ( 'NONE', *, *, #8519, .F. ) ;
#10306 = VECTOR ( 'NONE', #237, 999.9999999999998863 ) ;
#10307 = CARTESIAN_POINT ( 'NONE',  ( -10.16296170546024058, -21.54789006923565964, 6.318196777486344053E-14 ) ) ;
#10308 = ORIENTED_EDGE ( 'NONE', *, *, #15118, .F. ) ;
#10309 = CARTESIAN_POINT ( 'NONE',  ( -10.75228648362910100, -26.64274437364854009, 37.51367750791695954 ) ) ;
#10310 = EDGE_CURVE ( 'NONE', #8594, #13407, #10880, .T. ) ;
#10311 = DIRECTION ( 'NONE',  ( 0.000000000000000000, 0.000000000000000000, -1.000000000000000000 ) ) ;
#10312 = CARTESIAN_POINT ( 'NONE',  ( -1.767766952966370209, 65.76776695296638309, 45.20000000218494307 ) ) ;
#10313 = CARTESIAN_POINT ( 'NONE',  ( -41.00000000000000711, 53.00000000000000711, 0.5000000000000004441 ) ) ;
#10314 = DIRECTION ( 'NONE',  ( -1.000000000000000000, -0.000000000000000000, -0.000000000000000000 ) ) ;
#10315 = CARTESIAN_POINT ( 'NONE',  ( -1.530808498934192803E-16, 66.50000000000000000, 46.59999999999999432 ) ) ;
#10316 = CARTESIAN_POINT ( 'NONE',  ( 1.461580736456473684, 65.46158073645646880, 47.05000000109247082 ) ) ;
#10317 = VECTOR ( 'NONE', #3437, 1000.000000000000000 ) ;
#10318 = CARTESIAN_POINT ( 'NONE',  ( -43.50000000000000711, 2.999000000000001442, -52.50000000000000711 ) ) ;
#10319 = CARTESIAN_POINT ( 'NONE',  ( 1.767766952966369987, 65.76776695296638309, 46.49999999999999289 ) ) ;
#10320 = DIRECTION ( 'NONE',  ( 1.000000000000000000, -0.000000000000000000, -0.000000000000000000 ) ) ;
#10321 = VECTOR ( 'NONE', #10603, 1000.000000000000000 ) ;
#10322 = ORIENTED_EDGE ( 'NONE', *, *, #476, .F. ) ;
#10323 =( NAMED_UNIT ( * ) SI_UNIT ( $, .STERADIAN. ) SOLID_ANGLE_UNIT ( ) );
#10324 = EDGE_CURVE ( 'NONE', #2359, #5477, #3540, .T. ) ;
#10325 = CARTESIAN_POINT ( 'NONE',  ( -15.16482700510259640, -28.99999999999998224, 6.888677507916957765 ) ) ;
#10326 = EDGE_CURVE ( 'NONE', #8595, #15143, #18551, .T. ) ;
#10327 = CARTESIAN_POINT ( 'NONE',  ( -9.999999999999994671, -24.16482700510257686, 16.07617750791695954 ) ) ;
#10328 = CARTESIAN_POINT ( 'NONE',  ( -1.530808498934192803E-16, 66.50000000000000000, 48.30000000218494449 ) ) ;
#10329 = EDGE_CURVE ( 'NONE', #8266, #763, #18641, .T. ) ;
#10330 = CARTESIAN_POINT ( 'NONE',  ( -10.04416526290808953, -22.49542703274172695, 7.330072492083041347 ) ) ;
#10331 = CIRCLE ( 'NONE', #9715, 4.000000000000000000 ) ;
#10332 = CARTESIAN_POINT ( 'NONE',  ( -2.066987300000001415, 64.00000000000000000, 45.75000000109247367 ) ) ;
#10333 = CARTESIAN_POINT ( 'NONE',  ( -19.99999999999999645, -23.83517299489738051, 8.201177507916957765 ) ) ;
#10334 = CARTESIAN_POINT ( 'NONE',  ( -9.999999999999994671, -24.16482700510257686, 10.82617750791695777 ) ) ;
#10335 = CARTESIAN_POINT ( 'NONE',  ( 2.500000000000001776, 64.00000000000000000, 48.79999999999999716 ) ) ;
#10336 = AXIS2_PLACEMENT_3D ( 'NONE', #12151, #3435, #5013 ) ;
#10337 = CARTESIAN_POINT ( 'NONE',  ( 11.00000000000000355, 0.000000000000000000, 1.219500000000000028 ) ) ;
#10338 = DIRECTION ( 'NONE',  ( 0.000000000000000000, 1.000000000000000000, 0.000000000000000000 ) ) ;
#10339 = CYLINDRICAL_SURFACE ( 'NONE', #11311, 1.500000000000000222 ) ;
#10340 = CIRCLE ( 'NONE', #11584, 2.041999999999999815 ) ;
#10341 = DIRECTION ( 'NONE',  ( 1.000000000000000000, 0.000000000000000000, 0.000000000000000000 ) ) ;
#10342 = FACE_OUTER_BOUND ( 'NONE', #6065, .T. ) ;
#10343 = VECTOR ( 'NONE', #10048, 1000.000000000000000 ) ;
#10344 = DIRECTION ( 'NONE',  ( -0.000000000000000000, 1.000000000000000000, -0.000000000000000000 ) ) ;
#10345 = VERTEX_POINT ( 'NONE', #10776 ) ;
#10346 = VERTEX_POINT ( 'NONE', #4924 ) ;
#10347 = CARTESIAN_POINT ( 'NONE',  ( -18.64274437364860049, -18.02023567606023491, 21.54882249208304046 ) ) ;
#10348 = SHAPE_REPRESENTATION_RELATIONSHIP ( 'NONE' , 'NONE' ,  #7269, #12712 ) ;
#10349 = ADVANCED_FACE ( 'NONE', ( #15407 ), #5118, .F. ) ;
#10350 = VECTOR ( 'NONE', #7633, 1000.000000000000000 ) ;
#10351 = DIRECTION ( 'NONE',  ( 1.000000000000000000, 0.000000000000000000, 2.973811673103096679E-16 ) ) ;
#10353 = ORIENTED_EDGE ( 'NONE', *, *, #4744, .T. ) ;
#10352 = ORIENTED_EDGE ( 'NONE', *, *, #11635, .F. ) ;
#10354 = PRODUCT_DEFINITION_SHAPE ( 'NONE', 'NONE',  #19397 ) ;
#10355 = CARTESIAN_POINT ( 'NONE',  ( -16.35725562635142794, -21.31951028609535470, 19.57617750791696309 ) ) ;
#10356 = DIRECTION ( 'NONE',  ( 0.000000000000000000, 0.000000000000000000, -1.000000000000000000 ) ) ;
#10357 = CARTESIAN_POINT ( 'NONE',  ( -14.83517299489734853, -30.99999999999998224, 3.611322492083039570 ) ) ;
#10358 = VECTOR ( 'NONE', #15720, 1000.000000000000000 ) ;
#10359 = FACE_OUTER_BOUND ( 'NONE', #14983, .T. ) ;
#10360 = CARTESIAN_POINT ( 'NONE',  ( -0.8561741729129465073, 61.93301270000000613, 48.90000000109247225 ) ) ;
#10361 = ORIENTED_EDGE ( 'NONE', *, *, #7940, .T. ) ;
#10362 = ORIENTED_EDGE ( 'NONE', *, *, #9670, .T. ) ;
#10363 = AXIS2_PLACEMENT_3D ( 'NONE', #13656, #239, #9633 ) ;
#10364 = DIRECTION ( 'NONE',  ( 0.000000000000000000, 0.000000000000000000, -1.000000000000000000 ) ) ;
#10365 = DIRECTION ( 'NONE',  ( 0.000000000000000000, 0.000000000000000000, -1.000000000000000000 ) ) ;
#10366 = ORIENTED_EDGE ( 'NONE', *, *, #9289, .F. ) ;
#10367 = CARTESIAN_POINT ( 'NONE',  ( -10.36397326697674437, -22.27655863311489171, -4.119453415160648062E-17 ) ) ;
#10368 = FACE_OUTER_BOUND ( 'NONE', #981, .T. ) ;
#10369 = CARTESIAN_POINT ( 'NONE',  ( 1.461580736456473906, 62.53841926354353120, 48.45000000109246940 ) ) ;
#10370 = DIRECTION ( 'NONE',  ( 0.000000000000000000, 0.000000000000000000, 1.000000000000000000 ) ) ;
#10371 = AXIS2_PLACEMENT_3D ( 'NONE', #13276, #9465, #10927 ) ;
#10372 = DIRECTION ( 'NONE',  ( 0.000000000000000000, 1.000000000000000000, 0.000000000000000000 ) ) ;
#10373 = EDGE_CURVE ( 'NONE', #9301, #15994, #6679, .T. ) ;
#10374 = ORIENTED_EDGE ( 'NONE', *, *, #4080, .F. ) ;
#10376 = ORIENTED_EDGE ( 'NONE', *, *, #4554, .F. ) ;
#10375 = ORIENTED_EDGE ( 'NONE', *, *, #6504, .T. ) ;
#10377 = CARTESIAN_POINT ( 'NONE',  ( -20.24501739517664234, -29.00369391078761439, 18.04492750791695954 ) ) ;
#10378 = AXIS2_PLACEMENT_3D ( 'NONE', #4781, #13775, #17630 ) ;
#10379 = PLANE ( 'NONE',  #5237 ) ;
#10380 = VERTEX_POINT ( 'NONE', #13922 ) ;
#10381 = ORIENTED_EDGE ( 'NONE', *, *, #9440, .T. ) ;
#10382 = CARTESIAN_POINT ( 'NONE',  ( -19.95583473709190514, -25.50457296725822687, 41.45507249208304046 ) ) ;
#10383 = CARTESIAN_POINT ( 'NONE',  ( -40.00000000000000711, 110.0000000000000000, 1.500000000000001332 ) ) ;
#10384 = FACE_OUTER_BOUND ( 'NONE', #12119, .T. ) ;
#10385 = EDGE_CURVE ( 'NONE', #8527, #3207, #17071, .T. ) ;
#10386 = VERTEX_POINT ( 'NONE', #9605 ) ;
#10387 = CARTESIAN_POINT ( 'NONE',  ( -17.68048971390461688, -25.35725562635141372, 7.763677507916960430 ) ) ;
#10388 = ORIENTED_EDGE ( 'NONE', *, *, #11381, .T. ) ;
#10389 = DIRECTION ( 'NONE',  ( -0.000000000000000000, -0.7071067811865456854, -0.7071067811865494601 ) ) ;
#10390 = ORIENTED_EDGE ( 'NONE', *, *, #13586, .T. ) ;
#10391 = LINE ( 'NONE', #5600, #7872 ) ;
#10392 = DIRECTION ( 'NONE',  ( -0.5773502691896282846, -0.8164965809277242581, 0.000000000000000000 ) ) ;
#10393 = VECTOR ( 'NONE', #150, 1000.000000000000000 ) ;
#10394 = CARTESIAN_POINT ( 'NONE',  ( -25.00000000000000000, 113.0000000000000000, -50.00000000000000000 ) ) ;
#10395 = SHAPE_DEFINITION_REPRESENTATION ( #13329, #7269 ) ;
#10396 = CARTESIAN_POINT ( 'NONE',  ( -24.00000000000000000, 53.00000000000000711, 14.50000000000000000 ) ) ;
#10397 = CARTESIAN_POINT ( 'NONE',  ( 2.500000000000006661, 65.03553390593272354, 48.04999999999999716 ) ) ;
#10398 = ADVANCED_FACE ( 'NONE', ( #9509 ), #16778, .F. ) ;
#10399 = CARTESIAN_POINT ( 'NONE',  ( -10.58745947852649927, -21.64274437364853654, 15.63867750791695777 ) ) ;
#10400 = CARTESIAN_POINT ( 'NONE',  ( 49.99999999999998579, 118.0000000000000142, 40.49999999999997868 ) ) ;
#10401 = ORIENTED_EDGE ( 'NONE', *, *, #18600, .F. ) ;
#10402 = CARTESIAN_POINT ( 'NONE',  ( -10.75228648362912232, -21.35725562635138530, 7.111322492083040459 ) ) ;
#10403 = CARTESIAN_POINT ( 'NONE',  ( -2.066987300000001859, 64.85617417291294373, 44.70000000109248361 ) ) ;
#10404 = CARTESIAN_POINT ( 'NONE',  ( -12.48433729119799196, -22.35725562635139596, 7.111322492083044011 ) ) ;
#10405 = LINE ( 'NONE', #1403, #1900 ) ;
#10406 = ORIENTED_EDGE ( 'NONE', *, *, #377, .T. ) ;
#10407 = CARTESIAN_POINT ( 'NONE',  ( -10.82721319696594442, -20.04049993200424140, 1.010946030694833753E-16 ) ) ;
#10408 = EDGE_LOOP ( 'NONE', ( #9313, #2093, #1486, #15575 ) ) ;
#10409 = CARTESIAN_POINT ( 'NONE',  ( -13.82508104294698192, -29.04416526290806644, 38.16992750791695244 ) ) ;
#10410 = CARTESIAN_POINT ( 'NONE',  ( 1.300000000000000044, -0.7390083445627225744, -1.279999999999999138 ) ) ;
#10411 = CARTESIAN_POINT ( 'NONE',  ( 1.035533905932739751, 61.50000000000000000, 45.44999999999999574 ) ) ;
#10412 = DIRECTION ( 'NONE',  ( 0.000000000000000000, 1.000000000000000000, -0.000000000000000000 ) ) ;
#10413 = DIRECTION ( 'NONE',  ( -1.000000000000000000, -0.000000000000000000, -0.000000000000000000 ) ) ;
#10414 = CARTESIAN_POINT ( 'NONE',  ( -1.461580736456473906, 65.46158073645646880, 45.65000000109247225 ) ) ;
#10415 = CARTESIAN_POINT ( 'NONE',  ( -24.00000000000000000, 110.0000000000000000, -45.00000000000000000 ) ) ;
#10416 = CARTESIAN_POINT ( 'NONE',  ( -1.035533905932738641, 66.50000000000000000, 45.84999999999998721 ) ) ;
#10417 = FACE_OUTER_BOUND ( 'NONE', #16659, .T. ) ;
#10418 = ORIENTED_EDGE ( 'NONE', *, *, #2054, .T. ) ;
#10419 = ADVANCED_FACE ( 'NONE', ( #14122 ), #12450, .F. ) ;
#10420 = EDGE_CURVE ( 'NONE', #17455, #5786, #2067, .T. ) ;
#10421 = CARTESIAN_POINT ( 'NONE',  ( -9.955834737091912245, -22.82508104294696594, 5.357427507916956877 ) ) ;
#10422 = CARTESIAN_POINT ( 'NONE',  ( -11.46040770435012668, -27.78091578003887463, 16.73242750791695954 ) ) ;
#10423 = DIRECTION ( 'NONE',  ( -1.000000000000000000, 0.000000000000000000, -0.000000000000000000 ) ) ;
#10424 = EDGE_CURVE ( 'NONE', #7725, #16789, #12642, .T. ) ;
#10425 = CARTESIAN_POINT ( 'NONE',  ( -19.95583473709190514, -25.50457296725822687, 4.705072492083039570 ) ) ;
#10426 = MANIFOLD_SOLID_BREP ( 'Hex', #5062 ) ;
#10427 = CARTESIAN_POINT ( 'NONE',  ( 1.461580736456473906, 62.53841926354353120, 45.25000000109247367 ) ) ;
#10428 = CARTESIAN_POINT ( 'NONE',  ( -10.75228648362910100, -26.64274437364854009, 0.7636775079169582092 ) ) ;
#10429 = APPLICATION_CONTEXT ( 'automotive_design' ) ;
#10430 = EDGE_CURVE ( 'NONE', #3236, #9583, #5293, .T. ) ;
#10431 = DIRECTION ( 'NONE',  ( 1.000000000000000000, -7.160938508832259686E-15, 7.660538869913580129E-15 ) ) ;
#10432 = CARTESIAN_POINT ( 'NONE',  ( -25.00000000000000000, 53.00000000000000711, -37.50000000000000711 ) ) ;
#10433 = LINE ( 'NONE', #8971, #2782 ) ;
#10434 = FACE_OUTER_BOUND ( 'NONE', #17972, .T. ) ;
#10435 = CARTESIAN_POINT ( 'NONE',  ( -41.00000000000000711, 110.0000000000000000, -37.50000000000000711 ) ) ;
#10436 = LINE ( 'NONE', #5848, #1306 ) ;
#10437 = CARTESIAN_POINT ( 'NONE',  ( 3.796994071234847710E-16, 61.93301269999999903, 45.95000000109246940 ) ) ;
#10438 = PLANE ( 'NONE',  #6912 ) ;
#10439 = EDGE_CURVE ( 'NONE', #12326, #15077, #5017, .T. ) ;
#10440 = VECTOR ( 'NONE', #8859, 1000.000000000000000 ) ;
#10441 = ORIENTED_EDGE ( 'NONE', *, *, #7119, .F. ) ;
#10442 = CARTESIAN_POINT ( 'NONE',  ( 2.500000000000000000, -2.357898499370432610, 3.252606517456513302E-15 ) ) ;
#10443 = ORIENTED_EDGE ( 'NONE', *, *, #18958, .T. ) ;
#10444 = ORIENTED_EDGE ( 'NONE', *, *, #2698, .T. ) ;
#10445 = CARTESIAN_POINT ( 'NONE',  ( -8.044165262908093084, -21.95952864787946979, 12.58007249208304046 ) ) ;
#10446 = CARTESIAN_POINT ( 'NONE',  ( 2.500000000000006661, 65.03553390593272354, 47.24999999999998579 ) ) ;
#10448 = VERTEX_POINT ( 'NONE', #18729 ) ;
#10447 = ORIENTED_EDGE ( 'NONE', *, *, #57, .F. ) ;
#10449 = EDGE_CURVE ( 'NONE', #5590, #10078, #17268, .T. ) ;
#10450 = CARTESIAN_POINT ( 'NONE',  ( -11.95583473709191047, -23.36097942780921954, 15.85742750791696309 ) ) ;
#10451 = CARTESIAN_POINT ( 'NONE',  ( -4.000000000000001776, 67.00000000000000000, 34.99999999999999289 ) ) ;
#10452 = CARTESIAN_POINT ( 'NONE',  ( -16.71081734191527346, -16.95583473709190159, 40.79492750791695244 ) ) ;
#10453 = CARTESIAN_POINT ( 'NONE',  ( -2.066987300000001415, 64.00000000000000000, 49.55000000109247082 ) ) ;
#10454 = CARTESIAN_POINT ( 'NONE',  ( 1.767766952966370653, 62.23223304703363112, 45.60000000218494165 ) ) ;
#10455 = EDGE_LOOP ( 'NONE', ( #8498, #8893, #2768, #18041 ) ) ;
#10456 = ORIENTED_EDGE ( 'NONE', *, *, #810, .T. ) ;
#10457 = STYLED_ITEM ( 'NONE', ( #7818 ), #4072 ) ;
#10458 = FACE_OUTER_BOUND ( 'NONE', #458, .T. ) ;
#10459 = CARTESIAN_POINT ( 'NONE',  ( -40.00000000000000711, 113.0000000000000000, -11.49999999999999645 ) ) ;
#10460 = ORIENTED_EDGE ( 'NONE', *, *, #13110, .T. ) ;
#10461 = CARTESIAN_POINT ( 'NONE',  ( -12.84660369577459882, -20.49551723709882012, 7.657166918419683734E-13 ) ) ;
#10462 = CARTESIAN_POINT ( 'NONE',  ( -41.00000000000000711, 110.0000000000000000, -24.49999999999999645 ) ) ;
#10463 = CARTESIAN_POINT ( 'NONE',  ( 0.8561741729129472844, 61.93301270000000613, 46.80000000109246372 ) ) ;
#10464 = ADVANCED_FACE ( 'NONE', ( #16062 ), #5395, .T. ) ;
#10465 = EDGE_CURVE ( 'NONE', #8045, #9490, #6949, .T. ) ;
#10466 = CARTESIAN_POINT ( 'NONE',  ( -40.00000000000000711, 110.0000000000000000, 30.00000000000000000 ) ) ;
#10467 = CARTESIAN_POINT ( 'NONE',  ( -3.400000000000017675, 29.65425233947097183, 56.47747564417432642 ) ) ;
#10468 = ORIENTED_EDGE ( 'NONE', *, *, #18776, .T. ) ;
#10470 = ORIENTED_EDGE ( 'NONE', *, *, #10575, .T. ) ;
#10469 = VERTEX_POINT ( 'NONE', #4007 ) ;
#10471 = ADVANCED_FACE ( 'NONE', ( #12734 ), #18914, .F. ) ;
#10472 = CARTESIAN_POINT ( 'NONE',  ( -20.24501739517664234, -29.00369391078761439, 23.29492750791695599 ) ) ;
#10473 =( GEOMETRIC_REPRESENTATION_CONTEXT ( 3 ) GLOBAL_UNCERTAINTY_ASSIGNED_CONTEXT ( ( #12170 ) ) GLOBAL_UNIT_ASSIGNED_CONTEXT ( ( #14950, #8572, #11798 ) ) REPRESENTATION_CONTEXT ( 'NONE', 'WORKASPACE' ) );
#10474 = DIRECTION ( 'NONE',  ( 1.000000000000000000, 0.000000000000000000, 9.251858538542970348E-17 ) ) ;
#10475 = EDGE_LOOP ( 'NONE', ( #6271, #15670, #5688, #19282 ) ) ;
#10476 = VECTOR ( 'NONE', #15631, 1000.000000000000000 ) ;
#10477 = VERTEX_POINT ( 'NONE', #17343 ) ;
#10478 = CARTESIAN_POINT ( 'NONE',  ( -17.07549068051208963, -26.31681416490115311, 14.76757249208304223 ) ) ;
#10479 = CARTESIAN_POINT ( 'NONE',  ( 32.49999999999998579, 0.000000000000000000, 24.99999999999998224 ) ) ;
#10480 = CARTESIAN_POINT ( 'NONE',  ( -1.035533905932738863, 61.50000000000000000, 47.05000000218494449 ) ) ;
#10481 = VERTEX_POINT ( 'NONE', #17531 ) ;
#10482 = CARTESIAN_POINT ( 'NONE',  ( -15.96867458239597326, -26.95583473709190159, 22.85742750791695954 ) ) ;
#10483 = CARTESIAN_POINT ( 'NONE',  ( -1.035533905932738641, 66.50000000000000000, 47.55000000218494449 ) ) ;
#10484 = ORIENTED_EDGE ( 'NONE', *, *, #9847, .F. ) ;
#10485 = DIRECTION ( 'NONE',  ( -0.000000000000000000, 0.000000000000000000, 1.000000000000000000 ) ) ;
#10486 = ORIENTED_EDGE ( 'NONE', *, *, #18880, .T. ) ;
#10487 = EDGE_CURVE ( 'NONE', #4412, #18230, #8608, .T. ) ;
#10488 = CARTESIAN_POINT ( 'NONE',  ( -32.50000000000000000, 47.00000000000000711, 15.00000000000000000 ) ) ;
#10489 = LINE ( 'NONE', #15114, #6439 ) ;
#10490 = AXIS2_PLACEMENT_3D ( 'NONE', #5583, #9797, #9613 ) ;
#10491 = DIRECTION ( 'NONE',  ( -1.000000000000000000, 0.000000000000000000, 0.000000000000000000 ) ) ;
#10492 = SHAPE_DEFINITION_REPRESENTATION ( #7392, #8522 ) ;
#10493 = CARTESIAN_POINT ( 'NONE',  ( 1.300000000000000044, 0.7390083445627193548, -1.280000000000000693 ) ) ;
#10494 = FACE_OUTER_BOUND ( 'NONE', #10606, .T. ) ;
#10495 = CARTESIAN_POINT ( 'NONE',  ( -16.50457296725820555, -28.95583473709189448, 22.85742750791695954 ) ) ;
#10496 = CARTESIAN_POINT ( 'NONE',  ( -25.00000000000001421, 0.000000000000000000, 47.49999999999997868 ) ) ;
#10497 = ORIENTED_EDGE ( 'NONE', *, *, #3921, .F. ) ;
#10498 = CARTESIAN_POINT ( 'NONE',  ( -9.999999999999994671, -23.83517299489734143, 23.29882249208304046 ) ) ;
#10499 = PRODUCT_RELATED_PRODUCT_CATEGORY ( 'part', '', ( #12163 ) ) ;
#10500 = VECTOR ( 'NONE', #5715, 1000.000000000000000 ) ;
#10501 = VECTOR ( 'NONE', #11217, 1000.000000000000000 ) ;
#10502 = CARTESIAN_POINT ( 'NONE',  ( -0.8561741729129465073, 61.93301270000000613, 45.70000000109248361 ) ) ;
#10503 = CARTESIAN_POINT ( 'NONE',  ( -18.04416526290808775, -23.36097942780924441, 5.142572492083044011 ) ) ;
#10504 = DIRECTION ( 'NONE',  ( 0.000000000000000000, 0.000000000000000000, -1.000000000000000000 ) ) ;
#10505 = EDGE_LOOP ( 'NONE', ( #2034, #11774, #681, #16665 ) ) ;
#10506 = CARTESIAN_POINT ( 'NONE',  ( -24.00000000000000000, 53.00000000000000711, -31.00000000000000000 ) ) ;
#10507 = EDGE_LOOP ( 'NONE', ( #9207, #3856, #14465, #17541, #17042, #10644 ) ) ;
#10508 = CARTESIAN_POINT ( 'NONE',  ( 34.99999999999999289, -6.000000000000000000, 47.49999999999997868 ) ) ;
#10509 = CARTESIAN_POINT ( 'NONE',  ( 44.99999999999997158, 3.000000000000000000, 55.00000000000000000 ) ) ;
#10510 = DIRECTION ( 'NONE',  ( 0.000000000000000000, -0.7071067811865493491, 0.7071067811865457964 ) ) ;
#10511 = CARTESIAN_POINT ( 'NONE',  ( 1.000000000000001332, -36.00000000000000711, 9.500000000000001776 ) ) ;
#10512 = CARTESIAN_POINT ( 'NONE',  ( 2.066987300000001859, 63.14382582708704916, 46.10000000109246798 ) ) ;
#10513 = VECTOR ( 'NONE', #10344, 1000.000000000000000 ) ;
#10514 = CIRCLE ( 'NONE', #11756, 2.500000000000000444 ) ;
#10515 = PRODUCT_DEFINITION_SHAPE ( 'NONE', 'NONE',  #19407 ) ;
#10516 = LINE ( 'NONE', #7688, #10440 ) ;
#10517 = CARTESIAN_POINT ( 'NONE',  ( 2.500000000000001776, 65.03553390593273775, 45.64999999999999147 ) ) ;
#10518 = CARTESIAN_POINT ( 'NONE',  ( -10.00000000000000000, -32.00000000000001421, 3.500000000000006661 ) ) ;
#10519 =( BOUNDED_CURVE ( )  B_SPLINE_CURVE ( 2, ( #4710, #15283, #4904, #16856, #18235, #1855, #7843, #15386, #13807 ),
 .UNSPECIFIED., .F., .F. ) 
 B_SPLINE_CURVE_WITH_KNOTS ( ( 3, 2, 2, 2, 3 ),
 ( 0.6428571428571429047, 0.6607142857142856984, 0.6785714285714286031, 0.6964285714285712858, 0.7142857142857141906 ),
 .UNSPECIFIED. ) 
 CURVE ( )  GEOMETRIC_REPRESENTATION_ITEM ( )  RATIONAL_B_SPLINE_CURVE ( ( 1.000000000000000000, 0.9238795325112867385, 1.000000000000000000, 0.9238795325112867385, 1.000000000000000000, 0.9238795325112867385, 1.000000000000000000, 0.9238795325112871826, 0.9999999999999995559 ) ) 
 REPRESENTATION_ITEM ( '' )  );
#10520 = ORIENTED_EDGE ( 'NONE', *, *, #18596, .F. ) ;
#10521 = DIRECTION ( 'NONE',  ( 0.000000000000000000, 0.000000000000000000, 1.000000000000000000 ) ) ;
#10522 = CARTESIAN_POINT ( 'NONE',  ( -10.75228648362910100, -26.64274437364854009, 0.7636775079169582092 ) ) ;
#10523 = CARTESIAN_POINT ( 'NONE',  ( -9.999999999999994671, -24.16482700510257686, 10.82617750791695777 ) ) ;
#10524 = FACE_OUTER_BOUND ( 'NONE', #9732, .T. ) ;
#10525 = CARTESIAN_POINT ( 'NONE',  ( -18.53959229564982536, -27.78091578003890660, 4.267572492083038682 ) ) ;
#10526 = CIRCLE ( 'NONE', #17111, 2.500000000000000444 ) ;
#10527 = VECTOR ( 'NONE', #19334, 1000.000000000000000 ) ;
#10528 = CARTESIAN_POINT ( 'NONE',  ( -1.265664690411616068E-16, 66.06698730000000808, 45.55000000109246372 ) ) ;
#10529 = CARTESIAN_POINT ( 'NONE',  ( -12.35725562635143682, -19.75228648362908501, 4.701177507916957765 ) ) ;
#10530 = DIRECTION ( 'NONE',  ( 0.000000000000000000, 0.000000000000000000, -1.000000000000000000 ) ) ;
#10531 = CARTESIAN_POINT ( 'NONE',  ( -9.955834737091912245, -22.82508104294696238, 15.85742750791695954 ) ) ;
#10532 = CARTESIAN_POINT ( 'NONE',  ( -32.50000000000001421, -6.000000000000000000, 44.99999999999997868 ) ) ;
#10533 = EDGE_CURVE ( 'NONE', #13491, #513, #984, .T. ) ;
#10534 = CARTESIAN_POINT ( 'NONE',  ( 5.799326430397230503, 29.83055285973283333, 56.65377616443626607 ) ) ;
#10535 = DIRECTION ( 'NONE',  ( -0.000000000000000000, -0.000000000000000000, -1.000000000000000000 ) ) ;
#10536 = EDGE_CURVE ( 'NONE', #6823, #18134, #1161, .T. ) ;
#10537 = LINE ( 'NONE', #8775, #3491 ) ;
#10538 = CARTESIAN_POINT ( 'NONE',  ( 0.8561741729129471734, 61.93301270000000613, 45.20000000109248361 ) ) ;
#10539 = ADVANCED_FACE ( 'NONE', ( #12919 ), #17162, .T. ) ;
#10540 = LINE ( 'NONE', #9364, #18358 ) ;
#10541 = COLOUR_RGB ( '', 0.66274510, 0.83137255, 0.94901961) ;
#10542 = DIRECTION ( 'NONE',  ( 0.000000000000000000, -0.000000000000000000, 1.000000000000000000 ) ) ;
#10543 = ORIENTED_EDGE ( 'NONE', *, *, #6435, .T. ) ;
#10544 = VERTEX_POINT ( 'NONE', #6766 ) ;
#10545 = CARTESIAN_POINT ( 'NONE',  ( -7.955834737091903364, -25.71081734191518464, 23.51757249208304401 ) ) ;
#10546 = EDGE_CURVE ( 'NONE', #14616, #3630, #10228, .T. ) ;
#10547 = SURFACE_SIDE_STYLE ('',( #8017 ) ) ;
#10548 = CARTESIAN_POINT ( 'NONE',  ( -15.00000000000000000, 35.00000000000000000, 0.000000000000000000 ) ) ;
#10550 = EDGE_LOOP ( 'NONE', ( #11955, #12702, #14992, #5585 ) ) ;
#10549 = ORIENTED_EDGE ( 'NONE', *, *, #10931, .T. ) ;
#10551 = CARTESIAN_POINT ( 'NONE',  ( -12.31951028609537602, -22.64274437364854364, 10.38867750791695954 ) ) ;
#10552 = CARTESIAN_POINT ( 'NONE',  ( -1.035533905932738863, 61.50000000000000000, 48.65000000218493881 ) ) ;
#10553 = CARTESIAN_POINT ( 'NONE',  ( -20.00369391078757886, -29.24501739517668142, 4.267572492083039570 ) ) ;
#10554 = CARTESIAN_POINT ( 'NONE',  ( 0.8561741729129472844, 61.93301270000000613, 49.00000000109246656 ) ) ;
#10555 = CARTESIAN_POINT ( 'NONE',  ( 0.8561741729129472844, 61.93301270000000613, 46.60000000109246088 ) ) ;
#10556 = ORIENTED_EDGE ( 'NONE', *, *, #12722, .F. ) ;
#10557 = VERTEX_POINT ( 'NONE', #2534 ) ;
#10558 = CYLINDRICAL_SURFACE ( 'NONE', #12861, 2.500000000000001776 ) ;
#10559 = DIRECTION ( 'NONE',  ( -6.672013369141567928E-17, 0.000000000000000000, 1.000000000000000000 ) ) ;
#10560 = EDGE_LOOP ( 'NONE', ( #5286, #9864, #11648, #14802 ) ) ;
#10561 = CARTESIAN_POINT ( 'NONE',  ( -25.00000000000001421, -6.000000000000000000, 47.49999999999997868 ) ) ;
#10562 = CARTESIAN_POINT ( 'NONE',  ( 24.99999999999999289, 107.3545527679194436, -47.50000000000002132 ) ) ;
#10563 = EDGE_CURVE ( 'NONE', #18251, #301, #8516, .T. ) ;
#10564 = CARTESIAN_POINT ( 'NONE',  ( 0.8561741729129460632, 66.06698729999999387, 47.10000000109246798 ) ) ;
#10565 = CARTESIAN_POINT ( 'NONE',  ( 0.000000000000000000, 0.000000000000000000, 45.00000000000000000 ) ) ;
#10566 = CARTESIAN_POINT ( 'NONE',  ( -24.00000000000000711, 110.0000000000000000, 8.000000000000000000 ) ) ;
#10567 = VERTEX_POINT ( 'NONE', #18821 ) ;
#10569 = ORIENTED_EDGE ( 'NONE', *, *, #14263, .T. ) ;
#10568 = ORIENTED_EDGE ( 'NONE', *, *, #16748, .T. ) ;
#10570 = CARTESIAN_POINT ( 'NONE',  ( -20.00369391078762860, -18.75498260482333279, 19.35742750791695954 ) ) ;
#10571 = CARTESIAN_POINT ( 'NONE',  ( -25.00000000000000711, 0.000000000000000000, -47.50000000000002132 ) ) ;
#10572 = ORIENTED_EDGE ( 'NONE', *, *, #16555, .T. ) ;
#10573 = ORIENTED_EDGE ( 'NONE', *, *, #9036, .F. ) ;
#10574 = CARTESIAN_POINT ( 'NONE',  ( -12.04416526290808420, -23.03132541760398766, 12.58007249208304401 ) ) ;
#10575 = EDGE_CURVE ( 'NONE', #5597, #12791, #14491, .T. ) ;
#10576 = EDGE_CURVE ( 'NONE', #14588, #2736, #7803, .T. ) ;
#10577 = CARTESIAN_POINT ( 'NONE',  ( -1.040834085586084257E-14, 30.44974746830581580, 47.55025253169416288 ) ) ;
#10578 = FACE_OUTER_BOUND ( 'NONE', #2024, .T. ) ;
#10579 = ORIENTED_EDGE ( 'NONE', *, *, #18638, .F. ) ;
#10580 = EDGE_CURVE ( 'NONE', #7648, #12574, #18851, .T. ) ;
#10581 = CARTESIAN_POINT ( 'NONE',  ( -12.04416526290807887, -24.96867458239596260, 16.29492750791696665 ) ) ;
#10582 = DIRECTION ( 'NONE',  ( -1.000000000000000000, -0.000000000000000000, -0.000000000000000000 ) ) ;
#10583 = ORIENTED_EDGE ( 'NONE', *, *, #4279, .F. ) ;
#10584 = DIRECTION ( 'NONE',  ( -1.156482317317871725E-16, 0.000000000000000000, 1.000000000000000000 ) ) ;
#10585 = ORIENTED_EDGE ( 'NONE', *, *, #12173, .F. ) ;
#10586 = CARTESIAN_POINT ( 'NONE',  ( 2.500000000000001776, 64.00000000000000000, 46.39999999999999858 ) ) ;
#10587 = DIRECTION ( 'NONE',  ( -1.000000000000000000, -0.000000000000000000, -0.000000000000000000 ) ) ;
#10588 = CARTESIAN_POINT ( 'NONE',  ( -3.400000000000020783, 29.65425233947096118, 56.83102903476758883 ) ) ;
#10589 = DIRECTION ( 'NONE',  ( 1.000000000000000000, 0.000000000000000000, 0.000000000000000000 ) ) ;
#10590 = CARTESIAN_POINT ( 'NONE',  ( -15.00000000000000000, 35.00000000000000000, 33.99999999999999289 ) ) ;
#10591 = CIRCLE ( 'NONE', #9029, 1.280000000000000027 ) ;
#10592 = CARTESIAN_POINT ( 'NONE',  ( -16.17491895705301275, -18.95583473709189803, 40.79492750791695954 ) ) ;
#10593 = FACE_OUTER_BOUND ( 'NONE', #1857, .T. ) ;
#10594 = CARTESIAN_POINT ( 'NONE',  ( -11.46040770435012668, -27.78091578003887463, 16.73242750791695954 ) ) ;
#10595 = DIRECTION ( 'NONE',  ( -0.000000000000000000, -0.000000000000000000, -1.000000000000000000 ) ) ;
#10596 = ORIENTED_EDGE ( 'NONE', *, *, #3850, .F. ) ;
#10597 = EDGE_CURVE ( 'NONE', #9604, #7944, #3296, .T. ) ;
#10598 = CARTESIAN_POINT ( 'NONE',  ( -18.53959229564982536, -27.78091578003890660, 20.01757249208304046 ) ) ;
#10599 = EDGE_CURVE ( 'NONE', #19340, #5563, #13210, .T. ) ;
#10600 = AXIS2_PLACEMENT_3D ( 'NONE', #17163, #10882, #12354 ) ;
#10601 = CARTESIAN_POINT ( 'NONE',  ( -11.99999999999999289, -23.83517299489735564, 18.04882249208304046 ) ) ;
#10602 = CIRCLE ( 'NONE', #16883, 1.280000000000000027 ) ;
#10603 = DIRECTION ( 'NONE',  ( 1.000000000000000000, 0.000000000000000000, 2.973811673103096679E-16 ) ) ;
#10604 = ORIENTED_EDGE ( 'NONE', *, *, #16680, .F. ) ;
#10605 = CARTESIAN_POINT ( 'NONE',  ( -41.00000000000000711, 53.00000000000000711, -18.00000000000000000 ) ) ;
#10606 = EDGE_LOOP ( 'NONE', ( #1748, #3872, #11720, #19121 ) ) ;
#10607 = FACE_OUTER_BOUND ( 'NONE', #6289, .T. ) ;
#10608 = PLANE ( 'NONE',  #18326 ) ;
#10609 = DIRECTION ( 'NONE',  ( -1.000000000000000000, 0.000000000000000000, -0.000000000000000000 ) ) ;
#10610 = CARTESIAN_POINT ( 'NONE',  ( 2.066987300000001415, 64.00000000000000000, 46.95000000109246940 ) ) ;
#10611 = DIRECTION ( 'NONE',  ( -1.000000000000000000, 0.000000000000000000, 0.000000000000000000 ) ) ;
#10612 = PLANE ( 'NONE',  #4438 ) ;
#10613 = DIRECTION ( 'NONE',  ( 0.000000000000000000, 0.000000000000000000, 1.000000000000000000 ) ) ;
#10614 = VECTOR ( 'NONE', #12179, 1000.000000000000000 ) ;
#10615 = VECTOR ( 'NONE', #1066, 1000.000000000000000 ) ;
#10616 = EDGE_CURVE ( 'NONE', #18125, #17611, #13673, .T. ) ;
#10617 = EDGE_LOOP ( 'NONE', ( #4802, #16886, #10376, #8525, #8625, #11954, #6920, #16737 ) ) ;
#10618 = DIRECTION ( 'NONE',  ( 0.000000000000000000, 1.000000000000000000, 0.000000000000000000 ) ) ;
#10619 = CARTESIAN_POINT ( 'NONE',  ( -19.41254052147348830, -26.35725562635142083, 13.01367750791695777 ) ) ;
#10620 = CARTESIAN_POINT ( 'NONE',  ( -12.35725562635143682, -19.75228648362908501, 9.951177507916959541 ) ) ;
#10621 = CARTESIAN_POINT ( 'NONE',  ( 1.767766952966370653, 62.23223304703363112, 48.80000000218494449 ) ) ;
#10622 = CARTESIAN_POINT ( 'NONE',  ( -10.58745947852648328, -26.35725562635138530, 23.73632249208304046 ) ) ;
#10623 = CARTESIAN_POINT ( 'NONE',  ( -0.08838834764832678714, 29.80514068711926257, 56.68014068711929809 ) ) ;
#10624 = CARTESIAN_POINT ( 'NONE',  ( -17.35725562635144215, -19.58745947852648683, 3.826177507916958209 ) ) ;
#10625 = CARTESIAN_POINT ( 'NONE',  ( -40.00000000000000711, 53.00000000000000711, -44.00000000000000000 ) ) ;
#10626 = CARTESIAN_POINT ( 'NONE',  ( -13.49542703274178201, -19.04416526290806289, 25.48242750791695244 ) ) ;
#10627 = VECTOR ( 'NONE', #3145, 1000.000000000000000 ) ;
#10628 = CARTESIAN_POINT ( 'NONE',  ( 5.000000000000007994, 60.00000000000000711, 69.99999999999998579 ) ) ;
#10629 = CARTESIAN_POINT ( 'NONE',  ( 0.8561741729129472844, 61.93301270000000613, 49.20000000109247651 ) ) ;
#10630 = CARTESIAN_POINT ( 'NONE',  ( -25.00000000000000711, 53.00000000000000711, 21.00000000000000000 ) ) ;
#10631 =( BOUNDED_CURVE ( )  B_SPLINE_CURVE ( 2, ( #6930, #18800, #8496, #15763, #11333, #2328, #15574, #761, #6741 ),
 .UNSPECIFIED., .F., .F. ) 
 B_SPLINE_CURVE_WITH_KNOTS ( ( 3, 2, 2, 2, 3 ),
 ( 0.3571428571428572618, 0.3750000000000000555, 0.3928571428571429047, 0.4107142857142856984, 0.4285714285714284921 ),
 .UNSPECIFIED. ) 
 CURVE ( )  GEOMETRIC_REPRESENTATION_ITEM ( )  RATIONAL_B_SPLINE_CURVE ( ( 0.9999999999999995559, 0.9238795325112871826, 1.000000000000000000, 0.9238795325112867385, 1.000000000000000000, 0.9238795325112867385, 1.000000000000000000, 0.9238795325112869605, 0.9999999999999997780 ) ) 
 REPRESENTATION_ITEM ( '' )  );
#10632 = LINE ( 'NONE', #16634, #1944 ) ;
#10633 = CIRCLE ( 'NONE', #1393, 0.9999999999999974465 ) ;
#10634 = CARTESIAN_POINT ( 'NONE',  ( -1.461580736456473906, 65.46158073645646880, 45.65000000109247225 ) ) ;
#10635 = DIRECTION ( 'NONE',  ( -1.000000000000000000, 0.000000000000000000, 0.000000000000000000 ) ) ;
#10636 = FACE_OUTER_BOUND ( 'NONE', #13227, .T. ) ;
#10637 = VECTOR ( 'NONE', #4478, 1000.000000000000000 ) ;
#10638 = DIRECTION ( 'NONE',  ( 1.000000000000000000, 0.000000000000000000, 0.000000000000000000 ) ) ;
#10639 = ORIENTED_EDGE ( 'NONE', *, *, #10695, .T. ) ;
#10640 = VERTEX_POINT ( 'NONE', #17727 ) ;
#10641 = CARTESIAN_POINT ( 'NONE',  ( -13.28918265808478694, -16.95583473709189093, 11.70507249208304046 ) ) ;
#10642 = AXIS2_PLACEMENT_3D ( 'NONE', #9611, #2077, #12739 ) ;
#10643 = CARTESIAN_POINT ( 'NONE',  ( -16.17491895705296656, -29.04416526290807354, 14.33007249208304046 ) ) ;
#10645 = ORIENTED_EDGE ( 'NONE', *, *, #2432, .F. ) ;
#10644 = ORIENTED_EDGE ( 'NONE', *, *, #8582, .F. ) ;
#10646 = CARTESIAN_POINT ( 'NONE',  ( -17.95583473709191580, -23.03132541760400898, 18.91992750791695954 ) ) ;
#10647 = CARTESIAN_POINT ( 'NONE',  ( -15.00000000000000000, 0.000000000000000000, 33.99999999999999289 ) ) ;
#10648 = CARTESIAN_POINT ( 'NONE',  ( -21.99999999999999289, -24.16482700510262305, 10.17382249208303868 ) ) ;
#10649 = AXIS2_PLACEMENT_3D ( 'NONE', #2870, #6112, #16299 ) ;
#10650 = CARTESIAN_POINT ( 'NONE',  ( 3.796994071234847710E-16, 61.93301269999999903, 48.95000000109246940 ) ) ;
#10651 = CARTESIAN_POINT ( 'NONE',  ( 3.796994071234847710E-16, 61.93301269999999903, 46.55000000109247082 ) ) ;
#10652 = ORIENTED_EDGE ( 'NONE', *, *, #6126, .T. ) ;
#10653 = ORIENTED_EDGE ( 'NONE', *, *, #11475, .F. ) ;
#10654 = CARTESIAN_POINT ( 'NONE',  ( 11.00000000000000355, 0.000000000000000000, 0.000000000000000000 ) ) ;
#10655 = ORIENTED_EDGE ( 'NONE', *, *, #8676, .T. ) ;
#10656 = VECTOR ( 'NONE', #2751, 1000.000000000000000 ) ;
#10657 = ORIENTED_EDGE ( 'NONE', *, *, #4892, .F. ) ;
#10658 = CARTESIAN_POINT ( 'NONE',  ( 0.8561741729129471734, 61.93301270000000613, 49.00000000109246656 ) ) ;
#10659 = CARTESIAN_POINT ( 'NONE',  ( 0.000000000000000000, 52.00000000000000711, -50.00000000000000000 ) ) ;
#10660 = AXIS2_PLACEMENT_3D ( 'NONE', #12008, #1438, #19280 ) ;
#10661 = CARTESIAN_POINT ( 'NONE',  ( -1.461580736456473462, 62.53841926354353120, 49.05000000109247082 ) ) ;
#10662 = CARTESIAN_POINT ( 'NONE',  ( 8.000000000000003553, -32.00000000000000711, 1.500000000000000000 ) ) ;
#10663 = VECTOR ( 'NONE', #4726, 1000.000000000000000 ) ;
#10664 = CARTESIAN_POINT ( 'NONE',  ( 1.035533905932738197, 66.50000000000000000, 47.45000000218494307 ) ) ;
#10665 = ORIENTED_EDGE ( 'NONE', *, *, #19337, .T. ) ;
#10667 = ORIENTED_EDGE ( 'NONE', *, *, #10324, .F. ) ;
#10666 = ORIENTED_EDGE ( 'NONE', *, *, #10236, .T. ) ;
#10668 = CARTESIAN_POINT ( 'NONE',  ( -9.020235676060220698, -27.64274437364852588, 16.51367750791695954 ) ) ;
#10669 = SURFACE_STYLE_USAGE ( .BOTH. , #9304 ) ;
#10670 = VECTOR ( 'NONE', #4330, 1000.000000000000000 ) ;
#10671 = EDGE_LOOP ( 'NONE', ( #15096, #2662, #2607, #990 ) ) ;
#10672 = ORIENTED_EDGE ( 'NONE', *, *, #8740, .T. ) ;
#10673 = CARTESIAN_POINT ( 'NONE',  ( -11.95583473709190514, -24.63902057219072361, 18.26757249208304401 ) ) ;
#10674 = EDGE_CURVE ( 'NONE', #2933, #5783, #9144, .T. ) ;
#10675 = EDGE_CURVE ( 'NONE', #6389, #13623, #252, .T. ) ;
#10676 = CARTESIAN_POINT ( 'NONE',  ( -22.04416526290807710, -25.71081734191525925, 2.732427507916957321 ) ) ;
#10677 = PRESENTATION_LAYER_ASSIGNMENT (  '', '', ( #1625 ) ) ;
#10678 = CARTESIAN_POINT ( 'NONE',  ( -0.8561741729129461742, 66.06698730000000808, 47.80000000109247082 ) ) ;
#10679 = CYLINDRICAL_SURFACE ( 'NONE', #1253, 2.649999999999992806 ) ;
#10680 = ORIENTED_EDGE ( 'NONE', *, *, #1634, .F. ) ;
#10681 = CARTESIAN_POINT ( 'NONE',  ( -12.92450931948788906, -26.31681416490114245, 16.73242750791696309 ) ) ;
#10682 = AXIS2_PLACEMENT_3D ( 'NONE', #4671, #4377, #13182 ) ;
#10683 = CARTESIAN_POINT ( 'NONE',  ( 7.500000000000005329, -38.00000000000000000, 4.500000000000000888 ) ) ;
#10684 = VERTEX_POINT ( 'NONE', #7909 ) ;
#10685 = CARTESIAN_POINT ( 'NONE',  ( -1.040834085586084257E-14, 21.25735931288069125, 56.74264068711926967 ) ) ;
#10686 = VERTEX_POINT ( 'NONE', #2729 ) ;
#10687 = CARTESIAN_POINT ( 'NONE',  ( 2.500000000000000000, 1.178949249685217193, 2.041999999999998483 ) ) ;
#10688 = FACE_BOUND ( 'NONE', #14726, .T. ) ;
#10689 = CARTESIAN_POINT ( 'NONE',  ( -32.50000000000001421, -6.000000000000000000, 44.99999999999997868 ) ) ;
#10690 = AXIS2_PLACEMENT_3D ( 'NONE', #4785, #3584, #9557 ) ;
#10691 = DIRECTION ( 'NONE',  ( 0.000000000000000000, 0.000000000000000000, 1.000000000000000000 ) ) ;
#10692 = CARTESIAN_POINT ( 'NONE',  ( -45.00000000000000000, 0.000000000000000000, 53.39999999999999147 ) ) ;
#10693 = VECTOR ( 'NONE', #19202, 1000.000000000000000 ) ;
#10694 = CARTESIAN_POINT ( 'NONE',  ( -17.35725562635144215, -19.58745947852648683, 35.32617750791695954 ) ) ;
#10695 = EDGE_CURVE ( 'NONE', #18430, #18471, #7491, .T. ) ;
#10696 = CARTESIAN_POINT ( 'NONE',  ( 24.00000000000000000, 47.00000000000000711, -50.00000000000000000 ) ) ;
#10697 = EDGE_LOOP ( 'NONE', ( #18609, #10556, #7237, #9694 ) ) ;
#10698 = ADVANCED_FACE ( 'NONE', ( #6237 ), #8700, .T. ) ;
#10699 = CARTESIAN_POINT ( 'NONE',  ( -13.82508104294698192, -29.04416526290806644, 22.41992750791695244 ) ) ;
#10700 = DIRECTION ( 'NONE',  ( 0.000000000000000000, 0.000000000000000000, -1.000000000000000000 ) ) ;
#10701 = ORIENTED_EDGE ( 'NONE', *, *, #19242, .T. ) ;
#10702 = CARTESIAN_POINT ( 'NONE',  ( -11.21908421996106320, -27.53959229564982181, 18.70507249208304401 ) ) ;
#10703 = APPLICATION_CONTEXT ( 'automotive_design' ) ;
#10704 = CARTESIAN_POINT ( 'NONE',  ( 0.000000000000000000, 0.000000000000000000, 0.000000000000000000 ) ) ;
#10705 = CARTESIAN_POINT ( 'NONE',  ( -17.95583473709190869, -24.96867458239598037, 25.70507249208304756 ) ) ;
#10706 = VECTOR ( 'NONE', #18491, 1000.000000000000000 ) ;
#10707 = DIRECTION ( 'NONE',  ( -0.5000000000000051070, 1.060575238724903217E-16, -0.8660254037844355990 ) ) ;
#10708 = ORIENTED_EDGE ( 'NONE', *, *, #1569, .T. ) ;
#10709 = CARTESIAN_POINT ( 'NONE',  ( 14.99999999999998579, 73.00000000000001421, 20.99999999999997513 ) ) ;
#10710 = VERTEX_POINT ( 'NONE', #16251 ) ;
#10711 = FACE_OUTER_BOUND ( 'NONE', #4791, .T. ) ;
#10712 = DIRECTION ( 'NONE',  ( -1.541976423090495880E-16, 0.000000000000000000, 1.000000000000000000 ) ) ;
#10713 = DIRECTION ( 'NONE',  ( -0.000000000000000000, -1.000000000000000000, -0.000000000000000000 ) ) ;
#10714 = FACE_BOUND ( 'NONE', #17420, .T. ) ;
#10715 = EDGE_CURVE ( 'NONE', #4614, #6374, #4869, .T. ) ;
#10716 = ADVANCED_FACE ( 'NONE', ( #15156, #14793, #3388, #13874, #13574, #155 ), #11639, .F. ) ;
#10717 = CARTESIAN_POINT ( 'NONE',  ( -32.50000000000000000, 47.00000000000000711, -35.00000000000000000 ) ) ;
#10718 =( NAMED_UNIT ( * ) PLANE_ANGLE_UNIT ( ) SI_UNIT ( $, .RADIAN. ) );
#10719 = DIRECTION ( 'NONE',  ( 0.000000000000000000, 0.000000000000000000, -1.000000000000000000 ) ) ;
#10720 = ORIENTED_EDGE ( 'NONE', *, *, #3941, .T. ) ;
#10721 = ADVANCED_FACE ( 'NONE', ( #354 ), #6341, .T. ) ;
#10722 = DIRECTION ( 'NONE',  ( 0.000000000000000000, 0.000000000000000000, 1.000000000000000000 ) ) ;
#10723 = CARTESIAN_POINT ( 'NONE',  ( -18.53959229564986799, -20.21908421996107563, 14.10742750791695777 ) ) ;
#10724 = CARTESIAN_POINT ( 'NONE',  ( -1.530808498934192803E-16, 66.50000000000000000, 45.90000000218494591 ) ) ;
#10725 = CARTESIAN_POINT ( 'NONE',  ( -9.999999999999994671, -23.83517299489734143, 23.29882249208304046 ) ) ;
#10726 = CARTESIAN_POINT ( 'NONE',  ( -9.120482147295685276E-15, 33.84386001800124433, 52.64142135623733054 ) ) ;
#10727 = CARTESIAN_POINT ( 'NONE',  ( -12.35725562635143682, -19.75228648362908501, 9.951177507916959541 ) ) ;
#10728 = LINE ( 'NONE', #15250, #15184 ) ;
#10729 = CARTESIAN_POINT ( 'NONE',  ( -15.16482700510259640, -28.99999999999998224, 17.38867750791695599 ) ) ;
#10730 = DIRECTION ( 'NONE',  ( -0.000000000000000000, -1.000000000000000000, -0.000000000000000000 ) ) ;
#10731 = CARTESIAN_POINT ( 'NONE',  ( -2.500000000000006661, 65.03553390593272354, 45.94999999999999574 ) ) ;
#10732 = EDGE_CURVE ( 'NONE', #6748, #18273, #9357, .T. ) ;
#10733 = CARTESIAN_POINT ( 'NONE',  ( -1.265664690411616068E-16, 66.06698730000000808, 46.35000000109246798 ) ) ;
#10734 = LINE ( 'NONE', #643, #4018 ) ;
#10735 = DIRECTION ( 'NONE',  ( 1.000000000000000000, -0.000000000000000000, -0.000000000000000000 ) ) ;
#10736 = CARTESIAN_POINT ( 'NONE',  ( -0.8561741729129461742, 66.06698730000000808, 45.60000000109246798 ) ) ;
#10737 = CARTESIAN_POINT ( 'NONE',  ( 2.066987300000002303, 63.14382582708705627, 47.70000000109247651 ) ) ;
#10738 = FACE_OUTER_BOUND ( 'NONE', #1985, .T. ) ;
#10739 = ORIENTED_EDGE ( 'NONE', *, *, #4698, .F. ) ;
#10740 = ORIENTED_EDGE ( 'NONE', *, *, #7940, .F. ) ;
#10741 = CARTESIAN_POINT ( 'NONE',  ( -16.71081734191520596, -31.04416526290808065, 35.33007249208304046 ) ) ;
#10742 = FILL_AREA_STYLE ('',( #12414 ) ) ;
#10743 = CARTESIAN_POINT ( 'NONE',  ( -18.53959229564983247, -27.78091578003891016, 4.267572492083039570 ) ) ;
#10744 = ORIENTED_EDGE ( 'NONE', *, *, #12432, .T. ) ;
#10745 = CARTESIAN_POINT ( 'NONE',  ( -15.96867458239597326, -26.95583473709190159, 17.60742750791696309 ) ) ;
#10746 = CARTESIAN_POINT ( 'NONE',  ( -11.25000000000000178, -35.50000000000000000, 5.500000000000000000 ) ) ;
#10747 = CARTESIAN_POINT ( 'NONE',  ( -14.83517299489734853, -30.99999999999998224, 14.11132249208304046 ) ) ;
#10748 = LINE ( 'NONE', #17926, #5400 ) ;
#10749 = CARTESIAN_POINT ( 'NONE',  ( -1.265664690411616068E-16, 66.06698730000000808, 45.35000000109246798 ) ) ;
#10750 = ORIENTED_EDGE ( 'NONE', *, *, #867, .F. ) ;
#10751 = EDGE_LOOP ( 'NONE', ( #9902, #5075, #10050, #14208 ) ) ;
#10752 = LINE ( 'NONE', #16657, #4721 ) ;
#10753 = DIRECTION ( 'NONE',  ( 0.000000000000000000, -1.000000000000000000, 1.026972870230479989E-15 ) ) ;
#10754 = ORIENTED_EDGE ( 'NONE', *, *, #6309, .F. ) ;
#10755 = CARTESIAN_POINT ( 'NONE',  ( 1.461580736456473684, 65.46158073645646880, 48.45000000109247651 ) ) ;
#10756 = CARTESIAN_POINT ( 'NONE',  ( -41.00000000000000711, 53.00000000000000711, 27.50000000000000000 ) ) ;
#10757 = CARTESIAN_POINT ( 'NONE',  ( -2.066987300000001859, 64.85617417291294373, 45.70000000109248361 ) ) ;
#10758 = CARTESIAN_POINT ( 'NONE',  ( -25.00000000000000711, 53.00000000000000711, 13.50000000000000000 ) ) ;
#10759 = ORIENTED_EDGE ( 'NONE', *, *, #4171, .F. ) ;
#10761 = VERTEX_POINT ( 'NONE', #4205 ) ;
#10760 = EDGE_LOOP ( 'NONE', ( #12315, #7456 ) ) ;
#10762 = CARTESIAN_POINT ( 'NONE',  ( -13.28918265808472299, -31.04416526290805933, 11.91992750791695777 ) ) ;
#10763 = ORIENTED_EDGE ( 'NONE', *, *, #17851, .F. ) ;
#10764 = ORIENTED_EDGE ( 'NONE', *, *, #7308, .T. ) ;
#10765 = CARTESIAN_POINT ( 'NONE',  ( -13.64274437364857739, -21.31951028609534760, 17.17382249208304401 ) ) ;
#10766 = CARTESIAN_POINT ( 'NONE',  ( -22.04416526290807710, -25.71081734191525925, 13.23242750791695777 ) ) ;
#10767 =( GEOMETRIC_REPRESENTATION_CONTEXT ( 3 ) GLOBAL_UNCERTAINTY_ASSIGNED_CONTEXT ( ( #2192 ) ) GLOBAL_UNIT_ASSIGNED_CONTEXT ( ( #3374, #7894, #15529 ) ) REPRESENTATION_CONTEXT ( 'NONE', 'WORKASPACE' ) );
#10768 = CARTESIAN_POINT ( 'NONE',  ( 2.066987300000001859, 63.14382582708704916, 47.50000000109246656 ) ) ;
#10769 = PLANE ( 'NONE',  #331 ) ;
#10770 = ORIENTED_EDGE ( 'NONE', *, *, #1719, .F. ) ;
#10771 = CARTESIAN_POINT ( 'NONE',  ( -17.68048971390461688, -25.35725562635141372, 18.26367750791696309 ) ) ;
#10772 = LINE ( 'NONE', #14118, #15059 ) ;
#10773 = ORIENTED_EDGE ( 'NONE', *, *, #13911, .F. ) ;
#10774 = CARTESIAN_POINT ( 'NONE',  ( -1.035533905932738863, 61.50000000000000000, 45.34999999999998721 ) ) ;
#10775 = EDGE_LOOP ( 'NONE', ( #8823, #10401, #1669, #2417 ) ) ;
#10776 = CARTESIAN_POINT ( 'NONE',  ( -32.50000000000000000, 52.00000000000000711, -37.50000000000000711 ) ) ;
#10777 = CARTESIAN_POINT ( 'NONE',  ( -50.00000000000001421, 6.000000000000005329, 56.99999999999997158 ) ) ;
#10778 = DIRECTION ( 'NONE',  ( -3.491481338843133355E-15, -0.7071067811865495711, 0.7071067811865454633 ) ) ;
#10779 = DIRECTION ( 'NONE',  ( 0.000000000000000000, 1.000000000000000000, 0.000000000000000000 ) ) ;
#10780 = CARTESIAN_POINT ( 'NONE',  ( 4.012830983233625304, 26.60336399182260791, 59.52836399182266547 ) ) ;
#10781 = CONTEXT_DEPENDENT_SHAPE_REPRESENTATION ( #13059, #42 ) ;
#10782 = PLANE ( 'NONE',  #17115 ) ;
#10783 = CARTESIAN_POINT ( 'NONE',  ( -41.00000000000000711, 53.00000000000000711, 8.000000000000000000 ) ) ;
#10784 = ADVANCED_FACE ( 'NONE', ( #13070 ), #934, .T. ) ;
#10785 = ADVANCED_FACE ( 'NONE', ( #17599 ), #14269, .F. ) ;
#10786 = PRESENTATION_LAYER_ASSIGNMENT (  '', '', ( #1712 ) ) ;
#10787 = CARTESIAN_POINT ( 'NONE',  ( -2.500000000000001776, 64.00000000000000000, 46.90000000218494591 ) ) ;
#10788 = VECTOR ( 'NONE', #10712, 1000.000000000000000 ) ;
#10789 = CARTESIAN_POINT ( 'NONE',  ( 1.767766984964166399, 65.76776692096858312, 45.00000000000000000 ) ) ;
#10790 = ORIENTED_EDGE ( 'NONE', *, *, #3458, .T. ) ;
#10792 = ADVANCED_FACE ( 'NONE', ( #7107, #7009 ), #14555, .T. ) ;
#10791 = CARTESIAN_POINT ( 'NONE',  ( -17.64274437364855430, -28.24771351637087236, 17.82617750791695599 ) ) ;
#10793 = CARTESIAN_POINT ( 'NONE',  ( -40.00000000000000000, 53.00000000000000711, 26.50000000000000000 ) ) ;
#10794 = VERTEX_POINT ( 'NONE', #15751 ) ;
#10795 = PRODUCT_DEFINITION_CONTEXT ( 'detailed design', #8438, 'design' ) ;
#10796 = CARTESIAN_POINT ( 'NONE',  ( -11.46040770435014977, -20.21908421996103655, 12.14257249208304046 ) ) ;
#10797 = EDGE_CURVE ( 'NONE', #8383, #574, #9498, .T. ) ;
#10798 = CARTESIAN_POINT ( 'NONE',  ( -17.31681416490117087, -21.92450931948788551, 21.33007249208304401 ) ) ;
#10799 = AXIS2_PLACEMENT_3D ( 'NONE', #1218, #17658, #7365 ) ;
#10800 = SURFACE_SIDE_STYLE ('',( #15608 ) ) ;
#10801 = VERTEX_POINT ( 'NONE', #15840 ) ;
#10802 = VECTOR ( 'NONE', #15524, 1000.000000000000000 ) ;
#10803 = CARTESIAN_POINT ( 'NONE',  ( -24.00000000000000000, 110.0000000000000000, 26.50000000000000000 ) ) ;
#10804 = VERTEX_POINT ( 'NONE', #16124 ) ;
#10805 = DIRECTION ( 'NONE',  ( 0.000000000000000000, 0.000000000000000000, -1.000000000000000000 ) ) ;
#10806 = PLANE ( 'NONE',  #17688 ) ;
#10807 = DIRECTION ( 'NONE',  ( 0.000000000000000000, 0.000000000000000000, -1.000000000000000000 ) ) ;
#10808 = DIRECTION ( 'NONE',  ( -1.734723475976807094E-15, 1.000000000000000000, 0.000000000000000000 ) ) ;
#10809 = DIRECTION ( 'NONE',  ( 0.000000000000000000, 0.000000000000000000, 1.000000000000000000 ) ) ;
#10810 = DIRECTION ( 'NONE',  ( 0.000000000000000000, 0.000000000000000000, -1.000000000000000000 ) ) ;
#10811 = PLANE ( 'NONE',  #12087 ) ;
#10812 = VECTOR ( 'NONE', #6206, 1000.000000000000000 ) ;
#10813 = VECTOR ( 'NONE', #14691, 1000.000000000000000 ) ;
#10814 = UNCERTAINTY_MEASURE_WITH_UNIT (LENGTH_MEASURE( 1.000000000000000082E-05 ), #17192, 'distance_accuracy_value', 'NONE');
#10815 = ORIENTED_EDGE ( 'NONE', *, *, #12064, .F. ) ;
#10816 = CARTESIAN_POINT ( 'NONE',  ( 32.50000000000000000, 58.00000000000000000, 15.00000000000000000 ) ) ;
#10817 = CARTESIAN_POINT ( 'NONE',  ( -10.75228648362910100, -26.64274437364854009, 11.26367750791695777 ) ) ;
#10818 = CARTESIAN_POINT ( 'NONE',  ( 4.592425496802577917E-16, 61.50000000000000000, 45.50000000218494733 ) ) ;
#10819 = CARTESIAN_POINT ( 'NONE',  ( -11.46040770435014977, -20.21908421996103655, 12.14257249208304046 ) ) ;
#10820 = ADVANCED_FACE ( 'NONE', ( #13175 ), #3791, .F. ) ;
#10821 = ADVANCED_FACE ( 'NONE', ( #8386 ), #16035, .F. ) ;
#10822 = CARTESIAN_POINT ( 'NONE',  ( 0.1249999999999895917, 31.97002704785689531, 54.16170093578840294 ) ) ;
#10823 = CARTESIAN_POINT ( 'NONE',  ( -11.46040770435012668, -27.78091578003887463, 21.98242750791695244 ) ) ;
#10824 = EDGE_CURVE ( 'NONE', #15240, #13814, #2497, .T. ) ;
#10825 = CARTESIAN_POINT ( 'NONE',  ( -5.800000000000006928, 29.47747564417435484, 56.65425233947093631 ) ) ;
#10826 = VECTOR ( 'NONE', #15533, 1000.000000000000000 ) ;
#10827 = CARTESIAN_POINT ( 'NONE',  ( -17.35725562635144215, -19.58745947852648683, 19.57617750791695954 ) ) ;
#10828 = CARTESIAN_POINT ( 'NONE',  ( -25.00000000000000000, 53.00000000000000711, -45.00000000000000000 ) ) ;
#10829 = CARTESIAN_POINT ( 'NONE',  ( 0.000000000000000000, 3.000000000000000000, 0.000000000000000000 ) ) ;
#10830 = VECTOR ( 'NONE', #10121, 1000.000000000000000 ) ;
#10831 = EDGE_CURVE ( 'NONE', #7725, #17240, #8669, .T. ) ;
#10832 = CARTESIAN_POINT ( 'NONE',  ( 3.796994071234847710E-16, 61.93301269999999903, 47.55000000109247082 ) ) ;
#10833 = CARTESIAN_POINT ( 'NONE',  ( -6.528048594804060301, -45.28611686177728046, 3.000000000000000000 ) ) ;
#10834 = DIRECTION ( 'NONE',  ( 0.000000000000000000, 1.000000000000000000, -0.000000000000000000 ) ) ;
#10835 = CARTESIAN_POINT ( 'NONE',  ( 2.499999999999992895, 65.03553390593275196, 48.15000000218495302 ) ) ;
#10836 = CARTESIAN_POINT ( 'NONE',  ( 0.8561741729129472844, 61.93301270000000613, 48.40000000109247225 ) ) ;
#10837 = CARTESIAN_POINT ( 'NONE',  ( -25.00000000000000000, 110.0000000000000000, 30.00000000000000000 ) ) ;
#10838 = VERTEX_POINT ( 'NONE', #12888 ) ;
#10839 = ORIENTED_EDGE ( 'NONE', *, *, #5886, .T. ) ;
#10840 = CARTESIAN_POINT ( 'NONE',  ( -21.99999999999999289, -24.16482700510262305, 31.17382249208304046 ) ) ;
#10841 = VECTOR ( 'NONE', #14135, 1000.000000000000000 ) ;
#10842 = AXIS2_PLACEMENT_3D ( 'NONE', #2660, #11572, #6981 ) ;
#10843 = CARTESIAN_POINT ( 'NONE',  ( -19.99999999999999645, -24.16482700510261949, 10.17382249208304046 ) ) ;
#10844 = ORIENTED_EDGE ( 'NONE', *, *, #2088, .F. ) ;
#10845 = ADVANCED_FACE ( 'NONE', ( #14359 ), #8297, .F. ) ;
#10846 = CARTESIAN_POINT ( 'NONE',  ( -11.99999999999999289, -24.16482700510258752, 31.82617750791696309 ) ) ;
#10847 = ADVANCED_FACE ( 'NONE', ( #6820 ), #1034, .T. ) ;
#10848 = DIRECTION ( 'NONE',  ( 0.000000000000000000, 1.000000000000000000, 0.000000000000000000 ) ) ;
#10849 = CARTESIAN_POINT ( 'NONE',  ( -17.04047135212050890, -17.04416526290807710, 21.76757249208304401 ) ) ;
#10850 = CARTESIAN_POINT ( 'NONE',  ( 1.461580736456473906, 62.53841926354353120, 45.05000000109246372 ) ) ;
#10851 = CARTESIAN_POINT ( 'NONE',  ( 0.8561741729129460632, 66.06698729999999387, 47.70000000109248361 ) ) ;
#10852 = ORIENTED_EDGE ( 'NONE', *, *, #10616, .F. ) ;
#10853 = ORIENTED_EDGE ( 'NONE', *, *, #16339, .F. ) ;
#10854 = LINE ( 'NONE', #16849, #15621 ) ;
#10855 = CARTESIAN_POINT ( 'NONE',  ( -40.00000000000000711, 113.0000000000000000, 20.00000000000000000 ) ) ;
#10856 = ORIENTED_EDGE ( 'NONE', *, *, #3059, .F. ) ;
#10857 = CARTESIAN_POINT ( 'NONE',  ( -1.461580736456473462, 62.53841926354353120, 48.85000000109246798 ) ) ;
#10858 = LINE ( 'NONE', #9485, #15641 ) ;
#10859 = CIRCLE ( 'NONE', #15570, 1.599999999999997202 ) ;
#10860 = CARTESIAN_POINT ( 'NONE',  ( 2.066987300000002303, 63.14382582708705627, 45.30000000109247082 ) ) ;
#10861 = DIRECTION ( 'NONE',  ( -0.000000000000000000, 1.000000000000000000, -0.000000000000000000 ) ) ;
#10862 = DIRECTION ( 'NONE',  ( 0.000000000000000000, 0.000000000000000000, 1.000000000000000000 ) ) ;
#10863 = VERTEX_POINT ( 'NONE', #5546 ) ;
#10865 = EDGE_LOOP ( 'NONE', ( #2317, #320, #10246, #6092 ) ) ;
#10864 = ORIENTED_EDGE ( 'NONE', *, *, #17785, .T. ) ;
#10866 = CARTESIAN_POINT ( 'NONE',  ( -21.99999999999999289, -23.83517299489739116, 23.95117750791696309 ) ) ;
#10867 = ORIENTED_EDGE ( 'NONE', *, *, #12015, .T. ) ;
#10868 = EDGE_LOOP ( 'NONE', ( #7855, #5219, #2606, #9107 ) ) ;
#10869 = EDGE_CURVE ( 'NONE', #3171, #16792, #12883, .T. ) ;
#10870 = CARTESIAN_POINT ( 'NONE',  ( -11.99999999999999289, -23.83517299489735564, 28.54882249208304046 ) ) ;
#10871 = CARTESIAN_POINT ( 'NONE',  ( -11.64274437364854187, -30.14459132904234195, 22.20117750791695599 ) ) ;
#10872 =( BOUNDED_CURVE ( )  B_SPLINE_CURVE ( 2, ( #8450, #5603, #8359, #4033, #16001, #2563, #19135, #14518, #1089 ),
 .UNSPECIFIED., .F., .F. ) 
 B_SPLINE_CURVE_WITH_KNOTS ( ( 3, 2, 2, 2, 3 ),
 ( 0.2142857142857140795, 0.2321428571428570675, 0.2500000000000000000, 0.2678571428571429602, 0.2857142857142859205 ),
 .UNSPECIFIED. ) 
 CURVE ( )  GEOMETRIC_REPRESENTATION_ITEM ( )  RATIONAL_B_SPLINE_CURVE ( ( 1.000000000000000888, 0.9238795325112859613, 1.000000000000000000, 0.9238795325112867385, 1.000000000000000000, 0.9238795325112867385, 1.000000000000000000, 0.9238795325112857393, 1.000000000000000888 ) ) 
 REPRESENTATION_ITEM ( '' )  );
#10873 = DIRECTION ( 'NONE',  ( -1.000000000000000000, -2.312964634635742957E-16, 0.000000000000000000 ) ) ;
#10874 = CARTESIAN_POINT ( 'NONE',  ( 0.000000000000000000, -1.478016689125442706, 1.843143693225357538E-15 ) ) ;
#10875 = ORIENTED_EDGE ( 'NONE', *, *, #44, .T. ) ;
#10876 = CARTESIAN_POINT ( 'NONE',  ( -17.31681416490115311, -26.07549068051209318, 12.79492750791696132 ) ) ;
#10877 = ORIENTED_EDGE ( 'NONE', *, *, #19064, .F. ) ;
#10878 = CARTESIAN_POINT ( 'NONE',  ( -43.50000000000000000, 118.0000000000000142, 32.50000000000000000 ) ) ;
#10879 = EDGE_LOOP ( 'NONE', ( #11664, #15285, #5014, #1557 ) ) ;
#10880 = LINE ( 'NONE', #6292, #9737 ) ;
#10881 = CARTESIAN_POINT ( 'NONE',  ( 8.000000000000014211, 60.00000000000000711, 45.00000000000000000 ) ) ;
#10882 = DIRECTION ( 'NONE',  ( 0.000000000000000000, 0.000000000000000000, 1.000000000000000000 ) ) ;
#10883 = CARTESIAN_POINT ( 'NONE',  ( -32.50000000000002132, -6.000000000000000000, -25.00000000000002842 ) ) ;
#10884 = PLANE ( 'NONE',  #10150 ) ;
#10885 = CARTESIAN_POINT ( 'NONE',  ( -0.8561741729129465073, 61.93301270000000613, 48.10000000109246798 ) ) ;
#10886 = ITEM_DEFINED_TRANSFORMATION ( 'NONE', 'NONE', #7031,  #1791 ) ;
#10887 = CARTESIAN_POINT ( 'NONE',  ( 1.767766952966369987, 65.76776695296638309, 49.00000000218494023 ) ) ;
#10888 = FACE_OUTER_BOUND ( 'NONE', #13737, .T. ) ;
#10889 = CARTESIAN_POINT ( 'NONE',  ( 4.189607678530287593, 32.40336399182262284, 53.72836399182268252 ) ) ;
#10890 = DIRECTION ( 'NONE',  ( 0.000000000000000000, 0.000000000000000000, -1.000000000000000000 ) ) ;
#10891 = ORIENTED_EDGE ( 'NONE', *, *, #4238, .F. ) ;
#10892 = CARTESIAN_POINT ( 'NONE',  ( -19.95583473709191580, -22.49542703274176603, 29.41992750791695599 ) ) ;
#10893 = LINE ( 'NONE', #11085, #13983 ) ;
#10894 = ADVANCED_FACE ( 'NONE', ( #10037 ), #9844, .F. ) ;
#10895 = ORIENTED_EDGE ( 'NONE', *, *, #9289, .T. ) ;
#10896 = ADVANCED_FACE ( 'NONE', ( #10524 ), #4664, .F. ) ;
#10897 = CARTESIAN_POINT ( 'NONE',  ( -9.955834737091903364, -25.17491895705294880, 23.51757249208304401 ) ) ;
#10898 = CARTESIAN_POINT ( 'NONE',  ( -15.96867458239599635, -21.04416526290806999, 21.76757249208304756 ) ) ;
#10899 = DIRECTION ( 'NONE',  ( 0.000000000000000000, 0.000000000000000000, 1.000000000000000000 ) ) ;
#10900 = VERTEX_POINT ( 'NONE', #10233 ) ;
#10901 = CARTESIAN_POINT ( 'NONE',  ( -4.000000000000001776, 67.00000000000000000, 34.99999999999999289 ) ) ;
#10902 = ORIENTED_EDGE ( 'NONE', *, *, #4853, .F. ) ;
#10903 = DIRECTION ( 'NONE',  ( -0.000000000000000000, -0.000000000000000000, -1.000000000000000000 ) ) ;
#10904 = CARTESIAN_POINT ( 'NONE',  ( 2.749999999999979128, 118.0000000000000142, 40.49999999999995737 ) ) ;
#10905 = AXIS2_PLACEMENT_3D ( 'NONE', #15350, #451, #9651 ) ;
#10906 = PLANE ( 'NONE',  #14426 ) ;
#10907 = CARTESIAN_POINT ( 'NONE',  ( 0.8561741729129471734, 61.93301270000000613, 45.20000000109248361 ) ) ;
#10908 = DIRECTION ( 'NONE',  ( -0.000000000000000000, 1.000000000000000000, -0.000000000000000000 ) ) ;
#10909 = FILL_AREA_STYLE_COLOUR ( '', #671 ) ;
#10910 = EDGE_CURVE ( 'NONE', #3630, #17515, #4636, .T. ) ;
#10911 = CYLINDRICAL_SURFACE ( 'NONE', #1130, 2.999999999999999112 ) ;
#10912 = ORIENTED_EDGE ( 'NONE', *, *, #8994, .F. ) ;
#10913 = AXIS2_PLACEMENT_3D ( 'NONE', #18001, #6045, #15058 ) ;
#10914 = CARTESIAN_POINT ( 'NONE',  ( -9.999999999999994671, -24.16482700510257686, 21.32617750791695599 ) ) ;
#10915 = CARTESIAN_POINT ( 'NONE',  ( 2.500000000000001776, 65.03553390593273775, 45.75000000218494023 ) ) ;
#10916 = ADVANCED_FACE ( 'NONE', ( #2788 ), #117, .T. ) ;
#10917 = CARTESIAN_POINT ( 'NONE',  ( -9.955834737091903364, -25.17491895705294880, 18.26757249208304401 ) ) ;
#10918 = DIRECTION ( 'NONE',  ( -0.000000000000000000, -1.000000000000000000, -0.000000000000000000 ) ) ;
#10919 = CARTESIAN_POINT ( 'NONE',  ( -11.46040770435012668, -27.78091578003887463, 16.73242750791695954 ) ) ;
#10920 = CARTESIAN_POINT ( 'NONE',  ( -45.00000000000000000, 3.000000000000000000, 54.99999999999998579 ) ) ;
#10922 = CARTESIAN_POINT ( 'NONE',  ( -11.46040770435012490, -27.78091578003888173, 21.98242750791695244 ) ) ;
#10921 = VECTOR ( 'NONE', #11535, 1000.000000000000000 ) ;
#10923 = CARTESIAN_POINT ( 'NONE',  ( 47.00000000000000000, 118.0000000000000142, -56.99999999999999289 ) ) ;
#10924 = CARTESIAN_POINT ( 'NONE',  ( -15.16482700510263371, -18.99999999999997868, 27.23632249208304046 ) ) ;
#10925 = CARTESIAN_POINT ( 'NONE',  ( 0.8561741729129472844, 61.93301270000000613, 46.80000000109246372 ) ) ;
#10926 = CARTESIAN_POINT ( 'NONE',  ( 1.767766952966370653, 62.23223304703363112, 49.49999999999999289 ) ) ;
#10927 = DIRECTION ( 'NONE',  ( 0.000000000000000000, -0.7071067811865493491, 0.7071067811865457964 ) ) ;
#10928 = CARTESIAN_POINT ( 'NONE',  ( -25.00000000000000000, 53.00000000000000711, -50.00000000000000000 ) ) ;
#10929 = CARTESIAN_POINT ( 'NONE',  ( 2.066987300000001859, 64.85617417291294373, 47.80000000109247082 ) ) ;
#10930 = LINE ( 'NONE', #4877, #2667 ) ;
#10931 = EDGE_CURVE ( 'NONE', #885, #9861, #11860, .T. ) ;
#10932 = ORIENTED_EDGE ( 'NONE', *, *, #19039, .T. ) ;
#10933 = ORIENTED_EDGE ( 'NONE', *, *, #851, .T. ) ;
#10934 = EDGE_CURVE ( 'NONE', #16545, #3619, #17594, .T. ) ;
#10935 = CARTESIAN_POINT ( 'NONE',  ( -20.97976432393974022, -27.64274437364858628, 35.98632249208303335 ) ) ;
#10936 = VECTOR ( 'NONE', #14635, 1000.000000000000000 ) ;
#10937 = CARTESIAN_POINT ( 'NONE',  ( -13.49542703274174116, -28.95583473709188738, 13.89257249208304046 ) ) ;
#10938 = ORIENTED_EDGE ( 'NONE', *, *, #7698, .F. ) ;
#10939 = CARTESIAN_POINT ( 'NONE',  ( -14.03132541760401786, -21.04416526290806289, 35.98242750791695954 ) ) ;
#10940 = DIRECTION ( 'NONE',  ( 0.000000000000000000, 0.000000000000000000, -1.000000000000000000 ) ) ;
#10941 = CARTESIAN_POINT ( 'NONE',  ( -21.14459132904239169, -20.64274437364858628, 15.86132249208304223 ) ) ;
#10942 = VECTOR ( 'NONE', #11389, 1000.000000000000000 ) ;
#10943 = VECTOR ( 'NONE', #18732, 1000.000000000000000 ) ;
#10944 = CARTESIAN_POINT ( 'NONE',  ( 3.796994071234847710E-16, 61.93301269999999903, 45.75000000109247367 ) ) ;
#10945 = CARTESIAN_POINT ( 'NONE',  ( 1.461580736456473906, 62.53841926354353120, 46.65000000109247225 ) ) ;
#10946 = ORIENTED_EDGE ( 'NONE', *, *, #5431, .T. ) ;
#10947 = VERTEX_POINT ( 'NONE', #8846 ) ;
#10948 = DIRECTION ( 'NONE',  ( 0.000000000000000000, 1.632680918566406793E-16, -1.000000000000000000 ) ) ;
#10949 = CARTESIAN_POINT ( 'NONE',  ( -25.00000000000000711, 107.3545527679194436, -47.50000000000002132 ) ) ;
#10950 = CARTESIAN_POINT ( 'NONE',  ( -1.461580736456473906, 65.46158073645646880, 48.65000000109247225 ) ) ;
#10951 = LINE ( 'NONE', #5179, #6568 ) ;
#10952 = DIRECTION ( 'NONE',  ( 1.000000000000000000, 0.000000000000000000, 0.000000000000000000 ) ) ;
#10953 = AXIS2_PLACEMENT_3D ( 'NONE', #3602, #8488, #8120 ) ;
#10954 = LINE ( 'NONE', #2043, #8481 ) ;
#10955 = AXIS2_PLACEMENT_3D ( 'NONE', #9069, #4668, #15056 ) ;
#10956 = EDGE_CURVE ( 'NONE', #13224, #15564, #8138, .T. ) ;
#10957 = LINE ( 'NONE', #6270, #7691 ) ;
#10958 = ORIENTED_EDGE ( 'NONE', *, *, #6013, .F. ) ;
#10959 = ORIENTED_EDGE ( 'NONE', *, *, #16548, .T. ) ;
#10960 = CARTESIAN_POINT ( 'NONE',  ( -22.04416526290807710, -25.71081734191525925, 28.98242750791695599 ) ) ;
#10961 = ORIENTED_EDGE ( 'NONE', *, *, #5966, .F. ) ;
#10962 = VECTOR ( 'NONE', #10707, 1000.000000000000114 ) ;
#10963 = ORIENTED_EDGE ( 'NONE', *, *, #17399, .T. ) ;
#10964 = CARTESIAN_POINT ( 'NONE',  ( -17.95583473709190869, -24.96867458239598037, 30.95507249208304401 ) ) ;
#10965 = CARTESIAN_POINT ( 'NONE',  ( -20.00369391078762860, -18.75498260482333279, 19.35742750791695954 ) ) ;
#10966 = CIRCLE ( 'NONE', #1277, 1.280000000000000027 ) ;
#10967 = CARTESIAN_POINT ( 'NONE',  ( 1.461580736456473684, 65.46158073645646880, 47.65000000109247225 ) ) ;
#10968 = PLANE ( 'NONE',  #630 ) ;
#10969 = ORIENTED_EDGE ( 'NONE', *, *, #5201, .T. ) ;
#10970 = B_SPLINE_CURVE_WITH_KNOTS ( 'NONE', 1,
 ( #6162, #12219 ),
 .UNSPECIFIED., .F., .F.,
 ( 2, 2 ),
 ( 0.000000000000000000, 1.000000000000000000 ),
 .UNSPECIFIED. ) ;
#10971 = CARTESIAN_POINT ( 'NONE',  ( -15.63902057219076269, -20.95583473709189448, 35.54492750791696665 ) ) ;
#10972 = VECTOR ( 'NONE', #4437, 1000.000000000000000 ) ;
#10973 = EDGE_LOOP ( 'NONE', ( #2514, #7278, #14695, #10366 ) ) ;
#10974 = DIRECTION ( 'NONE',  ( 0.000000000000000000, -1.000000000000000000, 0.000000000000000000 ) ) ;
#10975 = ORIENTED_EDGE ( 'NONE', *, *, #7416, .F. ) ;
#10976 = DIRECTION ( 'NONE',  ( 1.000000000000000000, -0.000000000000000000, -0.000000000000000000 ) ) ;
#10977 = CARTESIAN_POINT ( 'NONE',  ( -37.50000000000002842, -6.000000000000000000, -47.50000000000002132 ) ) ;
#10978 = CARTESIAN_POINT ( 'NONE',  ( -24.00000000000000711, 110.0000000000000000, 21.00000000000000000 ) ) ;
#10979 = LINE ( 'NONE', #18261, #8599 ) ;
#10980 = CARTESIAN_POINT ( 'NONE',  ( 1.461580736456473906, 62.53841926354353120, 48.25000000109246656 ) ) ;
#10981 =( GEOMETRIC_REPRESENTATION_CONTEXT ( 3 ) GLOBAL_UNCERTAINTY_ASSIGNED_CONTEXT ( ( #13761 ) ) GLOBAL_UNIT_ASSIGNED_CONTEXT ( ( #7858, #17067, #2063 ) ) REPRESENTATION_CONTEXT ( 'NONE', 'WORKASPACE' ) );
#10982 = EDGE_CURVE ( 'NONE', #9890, #1607, #17960, .T. ) ;
#10983 = DIRECTION ( 'NONE',  ( 0.7071067811865463515, -0.5000000000000023315, 0.4999999999999994449 ) ) ;
#10984 = CARTESIAN_POINT ( 'NONE',  ( -7.999999999999996447, -25.00000000000000711, 1.500000000000000000 ) ) ;
#10985 = VECTOR ( 'NONE', #10952, 1000.000000000000000 ) ;
#10986 = CARTESIAN_POINT ( 'NONE',  ( -4.072081901468758147, 32.66337542264481186, 53.82127119883317334 ) ) ;
#10987 = PLANE ( 'NONE',  #9556 ) ;
#10988 = ORIENTED_EDGE ( 'NONE', *, *, #15306, .F. ) ;
#10989 = CARTESIAN_POINT ( 'NONE',  ( -12.64274437364855252, -28.41254052147347053, 32.70117750791696665 ) ) ;
#10990 =( BOUNDED_CURVE ( )  B_SPLINE_CURVE ( 2, ( #10304, #13548, #7380, #13645, #2963, #13352, #229, #8942, #9145 ),
 .UNSPECIFIED., .F., .F. ) 
 B_SPLINE_CURVE_WITH_KNOTS ( ( 3, 2, 2, 2, 3 ),
 ( 0.7142857142857141906, 0.7321428571428569843, 0.7500000000000000000, 0.7678571428571429047, 0.7857142857142856984 ),
 .UNSPECIFIED. ) 
 CURVE ( )  GEOMETRIC_REPRESENTATION_ITEM ( )  RATIONAL_B_SPLINE_CURVE ( ( 1.000000000000000444, 0.9238795325112862944, 1.000000000000000000, 0.9238795325112867385, 1.000000000000000000, 0.9238795325112867385, 1.000000000000000000, 0.9238795325112867385, 1.000000000000000000 ) ) 
 REPRESENTATION_ITEM ( '' )  );
#10991 = VECTOR ( 'NONE', #16138, 1000.000000000000000 ) ;
#10992 = DIRECTION ( 'NONE',  ( 0.000000000000000000, 0.000000000000000000, 1.000000000000000000 ) ) ;
#10993 = ORIENTED_EDGE ( 'NONE', *, *, #14966, .T. ) ;
#10994 = CARTESIAN_POINT ( 'NONE',  ( -17.64274437364858983, -19.75228648362910633, 37.29882249208303335 ) ) ;
#10995 = ADVANCED_FACE ( 'NONE', ( #11975 ), #18073, .F. ) ;
#10996 = CARTESIAN_POINT ( 'NONE',  ( -12.48433729119799196, -22.35725562635139596, 17.61132249208304401 ) ) ;
#10997 = DIRECTION ( 'NONE',  ( 0.000000000000000000, -0.6139406135149196864, 0.7893522173763268812 ) ) ;
#10998 = ORIENTED_EDGE ( 'NONE', *, *, #805, .F. ) ;
#10999 = AXIS2_PLACEMENT_3D ( 'NONE', #7914, #1827, #548 ) ;
#11000 = DIRECTION ( 'NONE',  ( 1.000000000000000000, -0.000000000000000000, 0.000000000000000000 ) ) ;
#11001 = ORIENTED_EDGE ( 'NONE', *, *, #2569, .T. ) ;
#11002 = PLANE ( 'NONE',  #2187 ) ;
#11003 = FACE_OUTER_BOUND ( 'NONE', #4740, .T. ) ;
#11004 = VECTOR ( 'NONE', #1725, 1000.000000000000000 ) ;
#11005 = CARTESIAN_POINT ( 'NONE',  ( -41.00000000000000711, 110.0000000000000000, -45.00000000000000000 ) ) ;
#11006 = FACE_BOUND ( 'NONE', #12641, .T. ) ;
#11007 = LINE ( 'NONE', #17008, #1705 ) ;
#11008 = DIRECTION ( 'NONE',  ( 0.000000000000000000, 0.000000000000000000, -1.000000000000000000 ) ) ;
#11009 = CARTESIAN_POINT ( 'NONE',  ( 0.000000000000000000, 0.000000000000000000, -50.00000000000000000 ) ) ;
#11010 = CARTESIAN_POINT ( 'NONE',  ( -41.00000000000000711, 110.0000000000000000, -32.00000000000000000 ) ) ;
#11011 = VECTOR ( 'NONE', #3152, 1000.000000000000000 ) ;
#11012 = ORIENTED_EDGE ( 'NONE', *, *, #2784, .T. ) ;
#11013 = VECTOR ( 'NONE', #4100, 1000.000000000000000 ) ;
#11014 = CARTESIAN_POINT ( 'NONE',  ( -19.24771351637089367, -21.35725562635142438, 13.88867750791695954 ) ) ;
#11015 = CARTESIAN_POINT ( 'NONE',  ( -2.500000000000001776, 64.00000000000000000, 45.30000000218493739 ) ) ;
#11016 = CARTESIAN_POINT ( 'NONE',  ( -11.21908421996106320, -27.53959229564982181, 13.45507249208304223 ) ) ;
#11017 = FACE_OUTER_BOUND ( 'NONE', #17552, .T. ) ;
#11018 = CARTESIAN_POINT ( 'NONE',  ( -18.78091578003889950, -27.53959229564985378, 18.04492750791695954 ) ) ;
#11019 = CARTESIAN_POINT ( 'NONE',  ( -40.00000000000000711, 113.0000000000000000, -5.000000000000004441 ) ) ;
#11020 = CARTESIAN_POINT ( 'NONE',  ( -9.955834737091912245, -22.82508104294696238, 36.85742750791696665 ) ) ;
#11021 = CARTESIAN_POINT ( 'NONE',  ( 1.767766952966370653, 62.23223304703363112, 47.09999999999999432 ) ) ;
#11022 = CARTESIAN_POINT ( 'NONE',  ( -9.955834737091903364, -25.17491895705295235, 18.26757249208304401 ) ) ;
#11023 = CARTESIAN_POINT ( 'NONE',  ( -1.461580736456473462, 62.53841926354353120, 47.45000000109246230 ) ) ;
#11024 = CARTESIAN_POINT ( 'NONE',  ( -41.00000000000000711, 53.00000000000000711, -5.000000000000000888 ) ) ;
#11025 = FACE_OUTER_BOUND ( 'NONE', #11348, .T. ) ;
#11026 = CARTESIAN_POINT ( 'NONE',  ( -41.00000000000000711, 53.00000000000000711, -37.50000000000000711 ) ) ;
#11027 = CARTESIAN_POINT ( 'NONE',  ( -0.8561741729129461742, 66.06698729999999387, 47.20000000109247651 ) ) ;
#11028 = EDGE_CURVE ( 'NONE', #1710, #15097, #862, .T. ) ;
#11029 = EDGE_CURVE ( 'NONE', #18716, #6167, #14205, .T. ) ;
#11030 = DIRECTION ( 'NONE',  ( 0.000000000000000000, 1.000000000000000000, 0.000000000000000000 ) ) ;
#11031 = EDGE_LOOP ( 'NONE', ( #17941, #16505, #10764, #6990 ) ) ;
#11032 = VERTEX_POINT ( 'NONE', #17061 ) ;
#11033 = CARTESIAN_POINT ( 'NONE',  ( -21.99999999999999289, -24.16482700510262305, 25.92382249208304046 ) ) ;
#11034 = EDGE_CURVE ( 'NONE', #10794, #11529, #11242, .T. ) ;
#11035 = FILL_AREA_STYLE ('',( #17311 ) ) ;
#11036 = CARTESIAN_POINT ( 'NONE',  ( -12.64274437364858628, -19.58745947852646552, 17.17382249208304401 ) ) ;
#11037 = CARTESIAN_POINT ( 'NONE',  ( -15.63902057219076269, -20.95583473709189448, 30.29492750791697020 ) ) ;
#11038 = CARTESIAN_POINT ( 'NONE',  ( -41.00000000000000711, 53.00000000000000711, 0.5000000000000004441 ) ) ;
#11039 = EDGE_CURVE ( 'NONE', #4427, #3539, #6574, .T. ) ;
#11040 = CARTESIAN_POINT ( 'NONE',  ( -9.996306089212408708, -18.75498260482328661, 17.39257249208304046 ) ) ;
#11041 = CARTESIAN_POINT ( 'NONE',  ( -2.066987300000001415, 63.14382582708705627, 47.20000000109248361 ) ) ;
#11042 = DIRECTION ( 'NONE',  ( 0.000000000000000000, 1.000000000000000000, 0.000000000000000000 ) ) ;
#11043 = VERTEX_POINT ( 'NONE', #9593 ) ;
#11044 = VERTEX_POINT ( 'NONE', #5283 ) ;
#11045 = CARTESIAN_POINT ( 'NONE',  ( -4.189607678530257395, 32.40336399182267257, 53.72836399182263278 ) ) ;
#11046 = CARTESIAN_POINT ( 'NONE',  ( 32.49999999999998579, -6.000000000000000000, 42.49999999999997868 ) ) ;
#11047 = PLANE ( 'NONE',  #283 ) ;
#11048 = CARTESIAN_POINT ( 'NONE',  ( -41.00000000000000000, 52.00000000000000711, 18.00000000000000000 ) ) ;
#11049 = EDGE_CURVE ( 'NONE', #3710, #10567, #14147, .T. ) ;
#11050 = CARTESIAN_POINT ( 'NONE',  ( 0.000000000000000000, 64.00000000000000000, 49.99999999999999289 ) ) ;
#11051 = CARTESIAN_POINT ( 'NONE',  ( -47.00000000000002132, 6.000000000000005329, -60.00000000000002132 ) ) ;
#11052 = CARTESIAN_POINT ( 'NONE',  ( 50.00000000000000000, 33.00000000000000000, 40.49999999999996447 ) ) ;
#11053 = EDGE_LOOP ( 'NONE', ( #11276, #13784, #6277, #18376 ) ) ;
#11054 = ADVANCED_FACE ( 'NONE', ( #9781, #686, #6755, #6670, #15774, #12633, #18812, #9142, #18630 ), #5386, .T. ) ;
#11055 = VERTEX_POINT ( 'NONE', #5197 ) ;
#11056 = CARTESIAN_POINT ( 'NONE',  ( -20.24501739517664234, -29.00369391078761439, 33.79492750791695244 ) ) ;
#11057 = ORIENTED_EDGE ( 'NONE', *, *, #18383, .F. ) ;
#11059 = ORIENTED_EDGE ( 'NONE', *, *, #14543, .F. ) ;
#11058 = ORIENTED_EDGE ( 'NONE', *, *, #1942, .F. ) ;
#11060 = CARTESIAN_POINT ( 'NONE',  ( -13.35725562635141195, -26.51566270880198672, 34.67382249208304756 ) ) ;
#11061 = CARTESIAN_POINT ( 'NONE',  ( -20.97976432393977575, -20.35725562635143504, 24.38867750791695954 ) ) ;
#11062 = DIRECTION ( 'NONE',  ( 1.156482317317871725E-16, 0.000000000000000000, -1.000000000000000000 ) ) ;
#11063 = CARTESIAN_POINT ( 'NONE',  ( 2.500000000000002220, 62.96446609406726935, 48.85000000218494165 ) ) ;
#11064 = PLANE ( 'NONE',  #8760 ) ;
#11065 = ORIENTED_EDGE ( 'NONE', *, *, #2293, .F. ) ;
#11066 = CARTESIAN_POINT ( 'NONE',  ( -11.95583473709191047, -23.36097942780921954, 31.60742750791695599 ) ) ;
#11067 = DIRECTION ( 'NONE',  ( -0.000000000000000000, 1.000000000000000000, 0.000000000000000000 ) ) ;
#11068 = EDGE_LOOP ( 'NONE', ( #12319, #6581, #15321, #10856 ) ) ;
#11069 = EDGE_CURVE ( 'NONE', #10640, #2931, #15128, .T. ) ;
#11070 = ADVANCED_FACE ( 'NONE', ( #18719 ), #3714, .T. ) ;
#11071 = CARTESIAN_POINT ( 'NONE',  ( -24.00000000000000711, 53.00000000000000711, -24.49999999999999645 ) ) ;
#11072 = ORIENTED_EDGE ( 'NONE', *, *, #15388, .F. ) ;
#11073 = DIRECTION ( 'NONE',  ( 0.000000000000000000, 0.000000000000000000, -1.000000000000000000 ) ) ;
#11074 = LINE ( 'NONE', #15409, #5032 ) ;
#11075 = DIRECTION ( 'NONE',  ( 0.000000000000000000, -1.000000000000000000, 0.000000000000000000 ) ) ;
#11076 = FACE_BOUND ( 'NONE', #12314, .T. ) ;
#11077 = CARTESIAN_POINT ( 'NONE',  ( 1.461580736456473684, 65.46158073645646880, 47.65000000109247225 ) ) ;
#11078 = EDGE_CURVE ( 'NONE', #2281, #16368, #1810, .T. ) ;
#11079 = CARTESIAN_POINT ( 'NONE',  ( 0.8561741729129471734, 61.93301270000000613, 47.60000000109246798 ) ) ;
#11080 = CARTESIAN_POINT ( 'NONE',  ( -41.00000000000000711, 53.00000000000000711, -45.00000000000000000 ) ) ;
#11081 = CARTESIAN_POINT ( 'NONE',  ( -45.00000000000000000, 3.000000000000000000, 53.49999999999998579 ) ) ;
#11082 = PLANE ( 'NONE',  #1430 ) ;
#11083 = ORIENTED_EDGE ( 'NONE', *, *, #4635, .T. ) ;
#11084 = CARTESIAN_POINT ( 'NONE',  ( -15.16482700510259640, -28.99999999999998224, 27.88867750791695954 ) ) ;
#11085 = CARTESIAN_POINT ( 'NONE',  ( 2.315774708385922587, 27.98014068711924551, 58.50514068711930804 ) ) ;
#11086 = EDGE_LOOP ( 'NONE', ( #2372, #11583, #5663, #1968 ) ) ;
#11087 = AXIS2_PLACEMENT_3D ( 'NONE', #9054, #3074, #10611 ) ;
#11088 = CARTESIAN_POINT ( 'NONE',  ( -12.64274437364858628, -19.58745947852646552, 32.92382249208304046 ) ) ;
#11089 = ADVANCED_BREP_SHAPE_REPRESENTATION ( '', ( #17097, #1791 ), #2707 ) ;
#11090 = EDGE_CURVE ( 'NONE', #12326, #5758, #12541, .T. ) ;
#11091 = CARTESIAN_POINT ( 'NONE',  ( -13.35725562635141195, -26.51566270880198672, 29.42382249208304401 ) ) ;
#11092 = DIRECTION ( 'NONE',  ( 0.000000000000000000, 0.000000000000000000, 1.000000000000000000 ) ) ;
#11093 = ORIENTED_EDGE ( 'NONE', *, *, #18361, .F. ) ;
#11094 = CARTESIAN_POINT ( 'NONE',  ( 43.50000000000001421, 118.0000000000000142, 32.49999999999998579 ) ) ;
#11095 = ORIENTED_EDGE ( 'NONE', *, *, #5730, .F. ) ;
#11096 = DIRECTION ( 'NONE',  ( -1.000000000000000000, 0.000000000000000000, 0.000000000000000000 ) ) ;
#11097 = CARTESIAN_POINT ( 'NONE',  ( -25.00000000000000711, 53.00000000000000711, -5.000000000000000888 ) ) ;
#11098 =( GEOMETRIC_REPRESENTATION_CONTEXT ( 3 ) GLOBAL_UNCERTAINTY_ASSIGNED_CONTEXT ( ( #4341 ) ) GLOBAL_UNIT_ASSIGNED_CONTEXT ( ( #4793, #9369, #171 ) ) REPRESENTATION_CONTEXT ( 'NONE', 'WORKASPACE' ) );
#11099 = LINE ( 'NONE', #9534, #668 ) ;
#11100 = AXIS2_PLACEMENT_3D ( 'NONE', #133, #9049, #10311 ) ;
#11101 = CARTESIAN_POINT ( 'NONE',  ( 1.035533905932738197, 66.50000000000000000, 46.54999999999999716 ) ) ;
#11102 = DIRECTION ( 'NONE',  ( 0.000000000000000000, 1.000000000000000000, 0.000000000000000000 ) ) ;
#11103 = FACE_BOUND ( 'NONE', #4453, .T. ) ;
#11104 = LINE ( 'NONE', #5048, #14574 ) ;
#11105 = ORIENTED_EDGE ( 'NONE', *, *, #18144, .F. ) ;
#11106 = PRODUCT_DEFINITION_FORMATION_WITH_SPECIFIED_SOURCE ( 'ANY', '', #10187, .NOT_KNOWN. ) ;
#11107 = CARTESIAN_POINT ( 'NONE',  ( -9.999999999999994671, -24.16482700510257686, 31.82617750791696309 ) ) ;
#11108 = VECTOR ( 'NONE', #998, 1000.000000000000000 ) ;
#11109 = ADVANCED_FACE ( 'NONE', ( #14294 ), #2250, .T. ) ;
#11110 = CARTESIAN_POINT ( 'NONE',  ( -2.500000000000000888, 62.96446609406726935, 45.35000000218493454 ) ) ;
#11111 = CARTESIAN_POINT ( 'NONE',  ( -10.04416526290808953, -22.49542703274172695, 28.33007249208304401 ) ) ;
#11112 = DIRECTION ( 'NONE',  ( 0.000000000000000000, 1.000000000000000000, 0.000000000000000000 ) ) ;
#11113 = CARTESIAN_POINT ( 'NONE',  ( -15.16482700510259640, -28.99999999999998224, 12.13867750791695777 ) ) ;
#11114 = FACE_OUTER_BOUND ( 'NONE', #15315, .T. ) ;
#11115 = CARTESIAN_POINT ( 'NONE',  ( -10.58745947852649927, -21.64274437364853654, 36.63867750791695954 ) ) ;
#11116 = DIRECTION ( 'NONE',  ( 0.000000000000000000, -1.000000000000000000, 0.000000000000000000 ) ) ;
#11117 = CARTESIAN_POINT ( 'NONE',  ( -14.83517299489735741, -28.99999999999998224, 19.36132249208304046 ) ) ;
#11118 = CARTESIAN_POINT ( 'NONE',  ( -1.767766952966370209, 65.76776695296638309, 49.89999999999999147 ) ) ;
#11119 = LINE ( 'NONE', #357, #2447 ) ;
#11120 = AXIS2_PLACEMENT_3D ( 'NONE', #7465, #4440, #8932 ) ;
#11121 = LINE ( 'NONE', #10096, #9750 ) ;
#11122 = AXIS2_PLACEMENT_3D ( 'NONE', #4973, #2021, #12111 ) ;
#11123 = LINE ( 'NONE', #17028, #7723 ) ;
#11124 = CARTESIAN_POINT ( 'NONE',  ( -0.8561741729129461742, 66.06698729999999387, 48.00000000109246656 ) ) ;
#11125 = DIRECTION ( 'NONE',  ( 0.000000000000000000, 0.000000000000000000, 1.000000000000000000 ) ) ;
#11126 = VERTEX_POINT ( 'NONE', #4750 ) ;
#11127 = CARTESIAN_POINT ( 'NONE',  ( -9.754982604823302594, -29.00369391078756465, 29.20507249208304046 ) ) ;
#11128 = CARTESIAN_POINT ( 'NONE',  ( -2.066987300000000971, 63.14382582708704916, 44.80000000109247082 ) ) ;
#11129 = CARTESIAN_POINT ( 'NONE',  ( -17.07549068051210739, -21.68318583509881847, 35.10742750791696665 ) ) ;
#11130 = PLANE ( 'NONE',  #12390 ) ;
#11131 = CARTESIAN_POINT ( 'NONE',  ( -9.020235676060250896, -20.35725562635137820, 12.36132249208304046 ) ) ;
#11132 = AXIS2_PLACEMENT_3D ( 'NONE', #1190, #3948, #17664 ) ;
#11133 = VECTOR ( 'NONE', #10613, 1000.000000000000000 ) ;
#11134 = CARTESIAN_POINT ( 'NONE',  ( 2.066987300000001859, 64.85617417291294373, 46.00000000109246656 ) ) ;
#11135 = VERTEX_POINT ( 'NONE', #18173 ) ;
#11136 = ORIENTED_EDGE ( 'NONE', *, *, #5325, .T. ) ;
#11137 = CARTESIAN_POINT ( 'NONE',  ( 7.500000000000005329, -38.00000000000000000, 4.500000000000000888 ) ) ;
#11138 = DIRECTION ( 'NONE',  ( -0.000000000000000000, -1.000000000000000000, -0.000000000000000000 ) ) ;
#11139 = CARTESIAN_POINT ( 'NONE',  ( -1.461580736456473906, 65.46158073645646880, 46.25000000109247367 ) ) ;
#11140 = DIRECTION ( 'NONE',  ( 1.000000000000000000, 0.000000000000000000, 0.000000000000000000 ) ) ;
#11141 = CARTESIAN_POINT ( 'NONE',  ( 2.066987300000001415, 64.00000000000000000, 45.35000000109246798 ) ) ;
#11142 = DIRECTION ( 'NONE',  ( -0.000000000000000000, 0.000000000000000000, 1.000000000000000000 ) ) ;
#11143 = EDGE_CURVE ( 'NONE', #5764, #8292, #16699, .T. ) ;
#11144 = VECTOR ( 'NONE', #812, 1000.000000000000000 ) ;
#11145 = CARTESIAN_POINT ( 'NONE',  ( 9.339266095310328808, -43.78611686177728046, 3.000000000000000000 ) ) ;
#11146 = ORIENTED_EDGE ( 'NONE', *, *, #1964, .T. ) ;
#11147 = VERTEX_POINT ( 'NONE', #5761 ) ;
#11148 = CARTESIAN_POINT ( 'NONE',  ( -16.71081734191527346, -16.95583473709190159, 35.54492750791695954 ) ) ;
#11149 = ORIENTED_EDGE ( 'NONE', *, *, #5697, .T. ) ;
#11151 = ORIENTED_EDGE ( 'NONE', *, *, #6639, .F. ) ;
#11150 = EDGE_LOOP ( 'NONE', ( #11059, #13904, #3527, #14488 ) ) ;
#11152 = CARTESIAN_POINT ( 'NONE',  ( -18.04416526290808775, -23.36097942780924441, 31.39257249208304401 ) ) ;
#11153 = CARTESIAN_POINT ( 'NONE',  ( -21.95583473709191580, -21.95952864787954084, 13.66992750791695954 ) ) ;
#11154 = CARTESIAN_POINT ( 'NONE',  ( 49.99999999999998579, 118.0000000000000142, 59.99999999999997868 ) ) ;
#11155 = CARTESIAN_POINT ( 'NONE',  ( 4.592425496802577917E-16, 61.50000000000000000, 47.10000000218494165 ) ) ;
#11156 = CARTESIAN_POINT ( 'NONE',  ( 32.50000000000000000, 52.00000000000000711, -37.50000000000000711 ) ) ;
#11157 = EDGE_LOOP ( 'NONE', ( #1501, #8132, #7238, #14570 ) ) ;
#11158 = CARTESIAN_POINT ( 'NONE',  ( -15.63902057219076269, -20.95583473709189448, 30.29492750791697020 ) ) ;
#11159 = ADVANCED_FACE ( 'NONE', ( #2614 ), #19194, .F. ) ;
#11160 = CARTESIAN_POINT ( 'NONE',  ( -50.00000000000002132, 3.000000000000000000, -60.00000000000002132 ) ) ;
#11161 = ORIENTED_EDGE ( 'NONE', *, *, #4354, .F. ) ;
#11162 = PRESENTATION_LAYER_ASSIGNMENT (  '', '', ( #17732 ) ) ;
#11163 = CARTESIAN_POINT ( 'NONE',  ( 4.189607678530260948, 26.72836399182260791, 59.40336399182267257 ) ) ;
#11164 = ORIENTED_EDGE ( 'NONE', *, *, #3136, .F. ) ;
#11165 = DIRECTION ( 'NONE',  ( 1.000000000000000000, -0.000000000000000000, -0.000000000000000000 ) ) ;
#11166 = CARTESIAN_POINT ( 'NONE',  ( -45.00000000000000000, 6.000000000000000000, 54.99999999999998579 ) ) ;
#11167 = CARTESIAN_POINT ( 'NONE',  ( 1.461580736456473684, 65.46158073645646880, 49.25000000109246656 ) ) ;
#11168 = CARTESIAN_POINT ( 'NONE',  ( -0.8561741729129466183, 61.93301270000000613, 46.70000000109248361 ) ) ;
#11169 = DIRECTION ( 'NONE',  ( -1.000000000000000000, -0.000000000000000000, -0.000000000000000000 ) ) ;
#11170 = CARTESIAN_POINT ( 'NONE',  ( -15.00000000000001421, -18.99999999999997868, 42.00000000000000000 ) ) ;
#11171 = CARTESIAN_POINT ( 'NONE',  ( 2.224021093614878986, 63.47751682961200004, 45.00000000000000711 ) ) ;
#11172 = ORIENTED_EDGE ( 'NONE', *, *, #2682, .F. ) ;
#11173 = VERTEX_POINT ( 'NONE', #17720 ) ;
#11174 = CARTESIAN_POINT ( 'NONE',  ( -11.21908421996108629, -20.46040770435011069, 36.41992750791695954 ) ) ;
#11175 = CARTESIAN_POINT ( 'NONE',  ( -40.00000000000000000, 52.00000000000000711, -50.00000000000000000 ) ) ;
#11176 = EDGE_CURVE ( 'NONE', #4727, #5670, #7130, .T. ) ;
#11177 = ORIENTED_EDGE ( 'NONE', *, *, #1250, .T. ) ;
#11178 = EDGE_CURVE ( 'NONE', #14286, #8292, #17429, .T. ) ;
#11179 = CARTESIAN_POINT ( 'NONE',  ( -17.64274437364858983, -19.75228648362910633, 32.04882249208304046 ) ) ;
#11180 = ADVANCED_FACE ( 'NONE', ( #5667 ), #11824, .T. ) ;
#11181 = CARTESIAN_POINT ( 'NONE',  ( -2.500000000000001776, 65.03553390593273775, 45.14999999999999858 ) ) ;
#11182 = CARTESIAN_POINT ( 'NONE',  ( -17.95583473709190869, -24.96867458239598037, 30.95507249208304401 ) ) ;
#11183 = LINE ( 'NONE', #18931, #13779 ) ;
#11184 = EDGE_LOOP ( 'NONE', ( #16373, #7918, #11440, #16464 ) ) ;
#11185 = LINE ( 'NONE', #8445, #16583 ) ;
#11186 = EDGE_LOOP ( 'NONE', ( #16263, #7079, #14155, #15197 ) ) ;
#11187 = FACE_OUTER_BOUND ( 'NONE', #6351, .T. ) ;
#11188 = PLANE ( 'NONE',  #9240 ) ;
#11189 = LINE ( 'NONE', #6415, #5666 ) ;
#11190 = EDGE_CURVE ( 'NONE', #2533, #10900, #5472, .T. ) ;
#11191 = DIRECTION ( 'NONE',  ( 0.000000000000000000, 1.000000000000000000, 0.000000000000000000 ) ) ;
#11192 = CARTESIAN_POINT ( 'NONE',  ( 32.50000000000000000, 47.00000000000000711, -35.00000000000000000 ) ) ;
#11193 = CARTESIAN_POINT ( 'NONE',  ( -3.065533689247737392, -43.60761626555502346, 3.000000000000000000 ) ) ;
#11194 = DIRECTION ( 'NONE',  ( 0.000000000000000000, 0.7071067811865452413, 0.7071067811865497932 ) ) ;
#11195 = UNCERTAINTY_MEASURE_WITH_UNIT (LENGTH_MEASURE( 1.000000000000000082E-05 ), #16965, 'distance_accuracy_value', 'NONE');
#11196 = ORIENTED_EDGE ( 'NONE', *, *, #19178, .F. ) ;
#11197 = CARTESIAN_POINT ( 'NONE',  ( -19.95583473709191580, -22.49542703274176603, 34.66992750791694533 ) ) ;
#11198 = CARTESIAN_POINT ( 'NONE',  ( -1.265664690411616068E-16, 66.06698730000000808, 49.35000000109246798 ) ) ;
#11199 = CARTESIAN_POINT ( 'NONE',  ( -9.999999999999994671, -23.83517299489734143, 33.79882249208304046 ) ) ;
#11200 = DIRECTION ( 'NONE',  ( -0.000000000000000000, -1.000000000000000000, -0.000000000000000000 ) ) ;
#11201 = CARTESIAN_POINT ( 'NONE',  ( -11.21908421996108629, -20.46040770435011069, 25.91992750791694888 ) ) ;
#11202 = FACE_OUTER_BOUND ( 'NONE', #1936, .T. ) ;
#11203 = CARTESIAN_POINT ( 'NONE',  ( -12.64274437364855252, -28.41254052147347053, 27.45117750791695954 ) ) ;
#11204 = DIRECTION ( 'NONE',  ( 0.000000000000000000, -1.000000000000000000, -0.000000000000000000 ) ) ;
#11205 = CARTESIAN_POINT ( 'NONE',  ( -19.24771351637086880, -26.64274437364857206, 30.73632249208304401 ) ) ;
#11206 = CARTESIAN_POINT ( 'NONE',  ( -1.767766952966370209, 65.76776695296638309, 49.09999999999999432 ) ) ;
#11207 = CARTESIAN_POINT ( 'NONE',  ( -5.800000000000005151, 29.74264068711930520, 56.74264068711926257 ) ) ;
#11208 = ADVANCED_FACE ( 'NONE', ( #9872 ), #17520, .F. ) ;
#11209 = CARTESIAN_POINT ( 'NONE',  ( 2.066987300000002303, 63.14382582708705627, 45.30000000109247082 ) ) ;
#11210 = CARTESIAN_POINT ( 'NONE',  ( 0.000000000000000000, 52.00000000000000711, 30.00000000000000000 ) ) ;
#11211 = VECTOR ( 'NONE', #2507, 1000.000000000000114 ) ;
#11212 = VERTEX_POINT ( 'NONE', #14582 ) ;
#11213 =( LENGTH_UNIT ( ) NAMED_UNIT ( * ) SI_UNIT ( .MILLI., .METRE. ) );
#11214 = CARTESIAN_POINT ( 'NONE',  ( 2.066987300000001415, 64.00000000000000000, 45.95000000109246940 ) ) ;
#11215 = CARTESIAN_POINT ( 'NONE',  ( -18.04416526290808420, -24.63902057219074493, 34.23242750791695954 ) ) ;
#11216 = EDGE_CURVE ( 'NONE', #292, #3881, #10060, .T. ) ;
#11217 = DIRECTION ( 'NONE',  ( -0.000000000000000000, -0.000000000000000000, -1.000000000000000000 ) ) ;
#11218 = CARTESIAN_POINT ( 'NONE',  ( -8.044165262908093084, -21.95952864787946979, 38.83007249208303335 ) ) ;
#11219 = VECTOR ( 'NONE', #7240, 1000.000000000000000 ) ;
#11220 = CARTESIAN_POINT ( 'NONE',  ( -1.461580736456473906, 65.46158073645646880, 45.45000000109246940 ) ) ;
#11221 = ORIENTED_EDGE ( 'NONE', *, *, #13455, .T. ) ;
#11222 = VECTOR ( 'NONE', #13774, 1000.000000000000000 ) ;
#11223 = LINE ( 'NONE', #15659, #15341 ) ;
#11224 = PLANE ( 'NONE',  #1302 ) ;
#11225 = CARTESIAN_POINT ( 'NONE',  ( 1.170854245699165075, 62.24769277278622326, 45.02598915381526012 ) ) ;
#11226 = DIRECTION ( 'NONE',  ( 0.000000000000000000, 0.000000000000000000, 1.000000000000000000 ) ) ;
#11227 = CARTESIAN_POINT ( 'NONE',  ( -1.767766952966370209, 65.76776695296638309, 49.20000000218494307 ) ) ;
#11228 = EDGE_CURVE ( 'NONE', #9159, #13243, #961, .T. ) ;
#11229 = LINE ( 'NONE', #8681, #3787 ) ;
#11230 = AXIS2_PLACEMENT_3D ( 'NONE', #17849, #4422, #4623 ) ;
#11231 = CARTESIAN_POINT ( 'NONE',  ( -37.50000000000002132, 0.000000000000000000, 24.99999999999998224 ) ) ;
#11232 = ORIENTED_EDGE ( 'NONE', *, *, #1564, .T. ) ;
#11233 = ORIENTED_EDGE ( 'NONE', *, *, #744, .T. ) ;
#11234 = CARTESIAN_POINT ( 'NONE',  ( -7.999999999999996447, -24.16482700510256976, 26.57617750791695954 ) ) ;
#11235 = ORIENTED_EDGE ( 'NONE', *, *, #15123, .T. ) ;
#11236 = CIRCLE ( 'NONE', #8133, 2.041999999999999815 ) ;
#11238 = ORIENTED_EDGE ( 'NONE', *, *, #14652, .T. ) ;
#11237 = ORIENTED_EDGE ( 'NONE', *, *, #9476, .F. ) ;
#11239 = CARTESIAN_POINT ( 'NONE',  ( -12.48433729119799196, -22.35725562635139596, 33.36132249208304756 ) ) ;
#11240 = CARTESIAN_POINT ( 'NONE',  ( -13.28918265808472299, -31.04416526290805933, 38.16992750791695954 ) ) ;
#11241 = AXIS2_PLACEMENT_3D ( 'NONE', #10153, #8602, #5570 ) ;
#11242 = LINE ( 'NONE', #18542, #3201 ) ;
#11243 = CARTESIAN_POINT ( 'NONE',  ( 1.767766952966369987, 65.76776695296638309, 46.60000000218494165 ) ) ;
#11244 = CARTESIAN_POINT ( 'NONE',  ( 1.300000000000000044, -1.478016689125442706, 1.843143693225357538E-15 ) ) ;
#11245 = ORIENTED_EDGE ( 'NONE', *, *, #3755, .T. ) ;
#11246 = CARTESIAN_POINT ( 'NONE',  ( -12.92450931948788906, -26.31681416490114245, 32.48242750791695954 ) ) ;
#11247 = AXIS2_PLACEMENT_3D ( 'NONE', #17185, #9722, #14328 ) ;
#11248 = CARTESIAN_POINT ( 'NONE',  ( -4.160453206537114923, 32.60057016663805740, 53.88344170207933104 ) ) ;
#11249 = VERTEX_POINT ( 'NONE', #12910 ) ;
#11250 = CARTESIAN_POINT ( 'NONE',  ( -15.00000000000001599, -18.99999999999997868, 0.000000000000000000 ) ) ;
#11251 = ORIENTED_EDGE ( 'NONE', *, *, #17189, .F. ) ;
#11252 = CARTESIAN_POINT ( 'NONE',  ( -50.00000000000002132, 30.00000000000000355, 43.75735931288070191 ) ) ;
#11253 = FACE_OUTER_BOUND ( 'NONE', #18015, .T. ) ;
#11254 = DIRECTION ( 'NONE',  ( 0.000000000000000000, 1.000000000000000000, 0.000000000000000000 ) ) ;
#11255 = VECTOR ( 'NONE', #4429, 1000.000000000000000 ) ;
#11256 = CARTESIAN_POINT ( 'NONE',  ( -1.461580736456473462, 62.53841926354353120, 46.45000000109246940 ) ) ;
#11257 = CARTESIAN_POINT ( 'NONE',  ( 2.066987300000001415, 64.00000000000000000, 49.35000000109246798 ) ) ;
#11258 = CARTESIAN_POINT ( 'NONE',  ( -41.00000000000000711, 53.00000000000000711, -45.00000000000000000 ) ) ;
#11259 =( BOUNDED_CURVE ( )  B_SPLINE_CURVE ( 2, ( #3781, #8663, #2686, #11495, #3869, #10026, #12969, #17483, #925 ),
 .UNSPECIFIED., .F., .F. ) 
 B_SPLINE_CURVE_WITH_KNOTS ( ( 3, 2, 2, 2, 3 ),
 ( 0.07142857142857156338, 0.08928571428571438484, 0.1071428571428571924, 0.1250000000000000000, 0.1428571428571428215 ),
 .UNSPECIFIED. ) 
 CURVE ( )  GEOMETRIC_REPRESENTATION_ITEM ( )  RATIONAL_B_SPLINE_CURVE ( ( 0.9999999999999994449, 0.9238795325112872936, 1.000000000000000000, 0.9238795325112867385, 1.000000000000000000, 0.9238795325112867385, 1.000000000000000000, 0.9238795325112868495, 0.9999999999999998890 ) ) 
 REPRESENTATION_ITEM ( '' )  );
#11260 = DIRECTION ( 'NONE',  ( -0.000000000000000000, 1.000000000000000000, -0.000000000000000000 ) ) ;
#11261 = MECHANICAL_DESIGN_GEOMETRIC_PRESENTATION_REPRESENTATION (  '', ( #4734 ), #2830 ) ;
#11262 = LINE ( 'NONE', #6686, #9251 ) ;
#11263 = ORIENTED_EDGE ( 'NONE', *, *, #13421, .F. ) ;
#11264 = ORIENTED_EDGE ( 'NONE', *, *, #17986, .F. ) ;
#11265 = EDGE_CURVE ( 'NONE', #17053, #11044, #13098, .T. ) ;
#11267 = EDGE_CURVE ( 'NONE', #7547, #4041, #8820, .T. ) ;
#11266 = CARTESIAN_POINT ( 'NONE',  ( -9.999999999999994671, -24.16482700510257686, 37.07617750791695954 ) ) ;
#11268 = DIRECTION ( 'NONE',  ( 0.000000000000000000, -0.7071067811865455743, -0.7071067811865495711 ) ) ;
#11269 = ORIENTED_EDGE ( 'NONE', *, *, #17781, .F. ) ;
#11270 = CARTESIAN_POINT ( 'NONE',  ( -19.24771351637086880, -26.64274437364857206, 35.98632249208304046 ) ) ;
#11271 = EDGE_CURVE ( 'NONE', #1736, #513, #8798, .T. ) ;
#11272 = CIRCLE ( 'NONE', #2511, 2.500000000000002220 ) ;
#11273 = CARTESIAN_POINT ( 'NONE',  ( 1.035533905932738197, 66.50000000000000000, 45.75000000000000000 ) ) ;
#11274 = CARTESIAN_POINT ( 'NONE',  ( -13.64274437364857739, -21.31951028609534760, 27.67382249208304401 ) ) ;
#11275 = CARTESIAN_POINT ( 'NONE',  ( -3.999999999999996447, 47.00000000000000711, 34.99999999999999289 ) ) ;
#11276 = ORIENTED_EDGE ( 'NONE', *, *, #16802, .F. ) ;
#11277 = AXIS2_PLACEMENT_3D ( 'NONE', #16017, #10013, #1199 ) ;
#11278 = CARTESIAN_POINT ( 'NONE',  ( -2.500000000000001776, 64.00000000000000000, 46.90000000218494591 ) ) ;
#11279 = VERTEX_POINT ( 'NONE', #1153 ) ;
#11280 = CARTESIAN_POINT ( 'NONE',  ( -24.00000000000000000, 110.0000000000000000, -19.00000000000000355 ) ) ;
#11281 = PLANE ( 'NONE',  #7364 ) ;
#11282 = CARTESIAN_POINT ( 'NONE',  ( -41.00000000000000711, 53.00000000000000711, 20.00000000000000000 ) ) ;
#11283 = VECTOR ( 'NONE', #2650, 1000.000000000000000 ) ;
#11284 = EDGE_CURVE ( 'NONE', #4512, #7552, #19002, .T. ) ;
#11285 = B_SPLINE_CURVE_WITH_KNOTS ( 'NONE', 3,
 ( #14987, #93, #1562, #191 ),
 .UNSPECIFIED., .F., .F.,
 ( 4, 4 ),
 ( 0.000000000000000000, 1.000000000000000000 ),
 .UNSPECIFIED. ) ;
#11286 = ADVANCED_FACE ( 'NONE', ( #2524 ), #17620, .T. ) ;
#11287 = EDGE_CURVE ( 'NONE', #3899, #17145, #10254, .T. ) ;
#11288 = CIRCLE ( 'NONE', #17566, 4.000000000000001776 ) ;
#11289 = LINE ( 'NONE', #12946, #9825 ) ;
#11290 = DIRECTION ( 'NONE',  ( 0.000000000000000000, 0.000000000000000000, 1.000000000000000000 ) ) ;
#11291 = FACE_OUTER_BOUND ( 'NONE', #6053, .T. ) ;
#11292 = PLANE ( 'NONE',  #13641 ) ;
#11293 = VECTOR ( 'NONE', #18150, 1000.000000000000000 ) ;
#11294 = ORIENTED_EDGE ( 'NONE', *, *, #1384, .F. ) ;
#11295 = VECTOR ( 'NONE', #6202, 1000.000000000000000 ) ;
#11296 = CARTESIAN_POINT ( 'NONE',  ( -13.49542703274178379, -19.04416526290806289, 35.98242750791696665 ) ) ;
#11297 = CARTESIAN_POINT ( 'NONE',  ( 1.461580736456473906, 62.53841926354353120, 46.65000000109247225 ) ) ;
#11298 = CARTESIAN_POINT ( 'NONE',  ( -9.999999999999994671, -23.83517299489734143, 39.04882249208304046 ) ) ;
#11299 = MECHANICAL_DESIGN_GEOMETRIC_PRESENTATION_REPRESENTATION (  '', ( #15086 ), #3498 ) ;
#11300 = CARTESIAN_POINT ( 'NONE',  ( 2.500000000000001776, 64.00000000000000000, 46.50000000218494733 ) ) ;
#11301 = CARTESIAN_POINT ( 'NONE',  ( -11.46040770435012668, -27.78091578003887463, 32.48242750791695954 ) ) ;
#11302 = VECTOR ( 'NONE', #6825, 1000.000000000000000 ) ;
#11303 = CARTESIAN_POINT ( 'NONE',  ( -15.00000000000000000, -32.50000000000001421, 3.328446124929187455 ) ) ;
#11304 = CARTESIAN_POINT ( 'NONE',  ( -10.04416526290807710, -25.50457296725819489, 37.29492750791695954 ) ) ;
#11305 = CARTESIAN_POINT ( 'NONE',  ( -2.749999999999989786, 38.00000000000000000, 37.49999999999995737 ) ) ;
#11306 = CARTESIAN_POINT ( 'NONE',  ( -16.50457296725825174, -19.04416526290807354, 21.76757249208304401 ) ) ;
#11307 = ADVANCED_FACE ( 'NONE', ( #14385 ), #4197, .F. ) ;
#11308 = EDGE_CURVE ( 'NONE', #12927, #17827, #14483, .T. ) ;
#11309 = CARTESIAN_POINT ( 'NONE',  ( 2.500000000000002220, 62.96446609406726935, 49.54999999999999716 ) ) ;
#11310 = CARTESIAN_POINT ( 'NONE',  ( 2.066987300000001415, 64.85617417291294373, 49.40000000109246514 ) ) ;
#11311 = AXIS2_PLACEMENT_3D ( 'NONE', #18005, #16229, #16136 ) ;
#11312 = CARTESIAN_POINT ( 'NONE',  ( -47.00000000000002132, 118.0000000000000142, -57.00000000000001421 ) ) ;
#11313 = EDGE_CURVE ( 'NONE', #8644, #2362, #16135, .T. ) ;
#11314 = CARTESIAN_POINT ( 'NONE',  ( -1.530808498934192803E-16, 66.50000000000000000, 49.79999999999999716 ) ) ;
#11315 = CARTESIAN_POINT ( 'NONE',  ( 1.753982408753060218, -46.96461745799954457, 3.000000000000000000 ) ) ;
#11316 = AXIS2_PLACEMENT_3D ( 'NONE', #8410, #13001, #3999 ) ;
#11317 = ORIENTED_EDGE ( 'NONE', *, *, #18832, .T. ) ;
#11318 = CARTESIAN_POINT ( 'NONE',  ( -0.1250000000000104083, 25.64142146683625612, 60.84290755733282197 ) ) ;
#11319 = CARTESIAN_POINT ( 'NONE',  ( -9.999999999999994671, -24.16482700510257686, 5.576177507916958653 ) ) ;
#11320 = DIRECTION ( 'NONE',  ( 0.000000000000000000, 0.000000000000000000, -1.000000000000000000 ) ) ;
#11321 = CARTESIAN_POINT ( 'NONE',  ( -11.64274437364859693, -17.85540867095757989, 27.67382249208304401 ) ) ;
#11322 = CARTESIAN_POINT ( 'NONE',  ( -2.066987300000001415, 64.00000000000000000, 48.15000000109247225 ) ) ;
#11323 = EDGE_CURVE ( 'NONE', #5562, #15859, #16353, .T. ) ;
#11324 = ORIENTED_EDGE ( 'NONE', *, *, #12135, .T. ) ;
#11325 = VECTOR ( 'NONE', #5934, 1000.000000000000000 ) ;
#11326 = CARTESIAN_POINT ( 'NONE',  ( 2.500000000000001776, 64.00000000000000000, 49.99999999999999289 ) ) ;
#11327 = PLANE ( 'NONE',  #1620 ) ;
#11328 = CARTESIAN_POINT ( 'NONE',  ( -2.066987300000000971, 63.14382582708704916, 47.20000000109248361 ) ) ;
#11329 = DIRECTION ( 'NONE',  ( -0.000000000000000000, -0.000000000000000000, -1.000000000000000000 ) ) ;
#11330 = DIRECTION ( 'NONE',  ( 0.000000000000000000, 0.000000000000000000, -1.000000000000000000 ) ) ;
#11331 = VECTOR ( 'NONE', #7735, 1000.000000000000000 ) ;
#11332 = DIRECTION ( 'NONE',  ( 0.000000000000000000, 1.000000000000000000, -1.224646799147353207E-16 ) ) ;
#11333 = CARTESIAN_POINT ( 'NONE',  ( 4.592425496802577917E-16, 61.50000000000000000, 47.79999999999999716 ) ) ;
#11334 = EDGE_LOOP ( 'NONE', ( #31, #1456, #8054, #18151 ) ) ;
#11335 = EDGE_LOOP ( 'NONE', ( #6567, #15263, #16343, #6800 ) ) ;
#11336 = CARTESIAN_POINT ( 'NONE',  ( -7.999999999999996447, -23.83517299489733432, 7.548822492083037794 ) ) ;
#11337 = SURFACE_STYLE_FILL_AREA ( #18996 ) ;
#11338 = VERTEX_POINT ( 'NONE', #11934 ) ;
#11340 = ORIENTED_EDGE ( 'NONE', *, *, #8362, .T. ) ;
#11339 = ORIENTED_EDGE ( 'NONE', *, *, #17357, .F. ) ;
#11341 = CARTESIAN_POINT ( 'NONE',  ( -11.99999999999999289, -24.16482700510258752, 5.576177507916960430 ) ) ;
#11342 = CARTESIAN_POINT ( 'NONE',  ( -12.95952864787955150, -17.04416526290805933, 25.48242750791696309 ) ) ;
#11343 = DIRECTION ( 'NONE',  ( 0.000000000000000000, -0.000000000000000000, -1.000000000000000000 ) ) ;
#11344 = CARTESIAN_POINT ( 'NONE',  ( -2.500000000000001776, 65.03553390593273775, 47.65000000218494591 ) ) ;
#11345 = DIRECTION ( 'NONE',  ( 0.000000000000000000, -0.7071067811865492381, 0.7071067811865457964 ) ) ;
#11346 = EDGE_LOOP ( 'NONE', ( #18903, #18884 ) ) ;
#11347 = CARTESIAN_POINT ( 'NONE',  ( -2.500000000000001776, 64.00000000000000000, 46.10000000218494165 ) ) ;
#11348 = EDGE_LOOP ( 'NONE', ( #11755, #3336, #12243, #15168 ) ) ;
#11349 = DIRECTION ( 'NONE',  ( 0.000000000000000000, 0.000000000000000000, -1.000000000000000000 ) ) ;
#11350 = ORIENTED_EDGE ( 'NONE', *, *, #13073, .F. ) ;
#11351 = CARTESIAN_POINT ( 'NONE',  ( 8.000000000000003553, 0.000000000000000000, 1.500000000000000000 ) ) ;
#11352 = CARTESIAN_POINT ( 'NONE',  ( -3.155775640247338920, -41.39960408384398249, 1.500000000000000000 ) ) ;
#11353 = CARTESIAN_POINT ( 'NONE',  ( -25.00000000000000000, 110.0000000000000000, 30.00000000000000000 ) ) ;
#11354 = CARTESIAN_POINT ( 'NONE',  ( 3.796994071234847710E-16, 61.93301269999999903, 44.95000000109246940 ) ) ;
#11355 = CARTESIAN_POINT ( 'NONE',  ( -50.00000000000001421, 118.0000000000000142, 56.99999999999997158 ) ) ;
#11356 = CARTESIAN_POINT ( 'NONE',  ( -10.00000000000000000, 49.99999999999997158, -4.956352788505161414E-14 ) ) ;
#11357 = CARTESIAN_POINT ( 'NONE',  ( -0.04165538583021200641, 25.64078660347668759, 60.84386001800125854 ) ) ;
#11358 = EDGE_LOOP ( 'NONE', ( #6577, #3898, #11898, #16478 ) ) ;
#11359 = ORIENTED_EDGE ( 'NONE', *, *, #14999, .F. ) ;
#11360 = CARTESIAN_POINT ( 'NONE',  ( -18.64274437364853654, -29.97976432393976509, 7.326177507916955989 ) ) ;
#11361 = DIRECTION ( 'NONE',  ( -3.826732013112564095E-16, 1.000000000000000000, 1.632680918566406793E-16 ) ) ;
#11362 = ORIENTED_EDGE ( 'NONE', *, *, #2682, .T. ) ;
#11363 = CARTESIAN_POINT ( 'NONE',  ( -17.35725562635140307, -28.41254052147349185, 30.29882249208304401 ) ) ;
#11364 = CARTESIAN_POINT ( 'NONE',  ( -1.035533905932738641, 66.50000000000000000, 45.84999999999998721 ) ) ;
#11365 = ORIENTED_EDGE ( 'NONE', *, *, #14519, .T. ) ;
#11366 = CARTESIAN_POINT ( 'NONE',  ( -14.36097942780925685, -20.95583473709189093, 32.70507249208304756 ) ) ;
#11367 = FACE_OUTER_BOUND ( 'NONE', #6372, .T. ) ;
#11368 = VERTEX_POINT ( 'NONE', #13593 ) ;
#11369 = DIRECTION ( 'NONE',  ( 0.000000000000000000, 0.000000000000000000, 1.000000000000000000 ) ) ;
#11370 = ORIENTED_EDGE ( 'NONE', *, *, #18991, .F. ) ;
#11371 = DIRECTION ( 'NONE',  ( 0.000000000000000000, 0.000000000000000000, -1.000000000000000000 ) ) ;
#11372 = EDGE_CURVE ( 'NONE', #14646, #9008, #4142, .T. ) ;
#11373 = EDGE_CURVE ( 'NONE', #13561, #19091, #10748, .T. ) ;
#11374 = CARTESIAN_POINT ( 'NONE',  ( 50.00000000000000000, 118.0000000000000142, 40.49999999999997868 ) ) ;
#11375 = DIRECTION ( 'NONE',  ( 0.000000000000000000, 0.000000000000000000, 1.000000000000000000 ) ) ;
#11376 = EDGE_CURVE ( 'NONE', #15564, #6663, #6062, .T. ) ;
#11377 = CARTESIAN_POINT ( 'NONE',  ( -10.75228648362910100, -26.64274437364854009, 32.26367750791695954 ) ) ;
#11378 = DIRECTION ( 'NONE',  ( 1.000000000000000000, 0.000000000000000000, 0.000000000000000000 ) ) ;
#11379 = DIRECTION ( 'NONE',  ( -1.000000000000000000, 0.000000000000000000, -0.000000000000000000 ) ) ;
#11381 = EDGE_CURVE ( 'NONE', #19221, #15669, #3198, .T. ) ;
#11380 = CARTESIAN_POINT ( 'NONE',  ( 32.50000000000000000, 0.000000000000000000, -42.49999999999999289 ) ) ;
#11382 = CARTESIAN_POINT ( 'NONE',  ( -3.400000000000017675, 29.65425233947097183, 56.47747564417432642 ) ) ;
#11383 = VERTEX_POINT ( 'NONE', #13793 ) ;
#11384 = UNCERTAINTY_MEASURE_WITH_UNIT (LENGTH_MEASURE( 1.000000000000000082E-05 ), #403, 'distance_accuracy_value', 'NONE');
#11385 = CARTESIAN_POINT ( 'NONE',  ( -10.58745947852649927, -21.64274437364853654, 36.63867750791695954 ) ) ;
#11386 = CARTESIAN_POINT ( 'NONE',  ( 1.461580736456473906, 62.53841926354353120, 48.25000000109246656 ) ) ;
#11387 = CARTESIAN_POINT ( 'NONE',  ( -19.41254052147350961, -21.64274437364857562, 26.36132249208304401 ) ) ;
#11388 = CARTESIAN_POINT ( 'NONE',  ( -2.499999999999984013, 62.96446609406724804, 48.45000000000000284 ) ) ;
#11389 = DIRECTION ( 'NONE',  ( 1.000000000000000000, 0.000000000000000000, 0.000000000000000000 ) ) ;
#11390 = CARTESIAN_POINT ( 'NONE',  ( -10.58745947852649927, -21.64274437364853654, 26.13867750791695599 ) ) ;
#11391 = ADVANCED_FACE ( 'NONE', ( #269 ), #12222, .T. ) ;
#11392 = DIRECTION ( 'NONE',  ( -0.000000000000000000, -1.000000000000000000, -0.000000000000000000 ) ) ;
#11393 = CARTESIAN_POINT ( 'NONE',  ( -19.99999999999999645, -23.83517299489738051, 34.45117750791696665 ) ) ;
#11394 = LINE ( 'NONE', #17388, #16243 ) ;
#11395 = CARTESIAN_POINT ( 'NONE',  ( 41.00000000000000000, 52.00000000000000711, -50.00000000000000000 ) ) ;
#11396 = CARTESIAN_POINT ( 'NONE',  ( -2.500000000000000888, 62.96446609406726935, 49.24999999999999289 ) ) ;
#11397 = CARTESIAN_POINT ( 'NONE',  ( -1.265664690411616068E-16, 66.06698730000000808, 48.75000000109246656 ) ) ;
#11398 = DIRECTION ( 'NONE',  ( -0.000000000000000000, 1.000000000000000000, -0.000000000000000000 ) ) ;
#11399 = CARTESIAN_POINT ( 'NONE',  ( -2.066987300000001859, 64.85617417291294373, 45.70000000109248361 ) ) ;
#11400 = CARTESIAN_POINT ( 'NONE',  ( -47.00000000000001421, 115.0000000000000000, 37.49999999999997868 ) ) ;
#11401 = VECTOR ( 'NONE', #17205, 1000.000000000000000 ) ;
#11402 = ORIENTED_EDGE ( 'NONE', *, *, #4485, .F. ) ;
#11403 = PRESENTATION_STYLE_ASSIGNMENT (( #12784 ) ) ;
#11404 = ADVANCED_FACE ( 'NONE', ( #10359 ), #4770, .T. ) ;
#11405 = CARTESIAN_POINT ( 'NONE',  ( 0.8561741729129460632, 66.06698730000000808, 46.90000000109247225 ) ) ;
#11406 = EDGE_CURVE ( 'NONE', #12225, #14571, #11998, .T. ) ;
#11407 = CARTESIAN_POINT ( 'NONE',  ( -16.64274437364856496, -26.51566270880199738, 38.82617750791695954 ) ) ;
#11408 = DIRECTION ( 'NONE',  ( 1.000000000000000000, 2.602085213965211135E-16, -0.000000000000000000 ) ) ;
#11409 = EDGE_CURVE ( 'NONE', #1646, #11598, #9066, .T. ) ;
#11410 = CARTESIAN_POINT ( 'NONE',  ( -16.71081734191520596, -31.04416526290808065, 35.33007249208304046 ) ) ;
#11411 = CARTESIAN_POINT ( 'NONE',  ( -1.265664690411616068E-16, 66.06698730000000808, 44.55000000109247082 ) ) ;
#11412 = ORIENTED_EDGE ( 'NONE', *, *, #16721, .F. ) ;
#11413 = PRODUCT_DEFINITION_FORMATION_WITH_SPECIFIED_SOURCE ( 'ANY', '', #11758, .NOT_KNOWN. ) ;
#11414 = CARTESIAN_POINT ( 'NONE',  ( 14.99999999999998579, 47.00000000000000711, 26.99999999999997158 ) ) ;
#11415 = CARTESIAN_POINT ( 'NONE',  ( 4.592425496802577917E-16, 61.50000000000000000, 45.50000000218494733 ) ) ;
#11416 = AXIS2_PLACEMENT_3D ( 'NONE', #12579, #15613, #1997 ) ;
#11417 = CARTESIAN_POINT ( 'NONE',  ( -1.265664690411616068E-16, 66.06698730000000808, 46.15000000109247225 ) ) ;
#11418 = DIRECTION ( 'NONE',  ( 2.775557561562891351E-16, 0.7071067811865454633, 0.7071067811865495711 ) ) ;
#11419 = PLANE ( 'NONE',  #5684 ) ;
#11420 = LINE ( 'NONE', #15944, #10991 ) ;
#11421 = DIRECTION ( 'NONE',  ( -0.000000000000000000, -1.000000000000000000, -0.000000000000000000 ) ) ;
#11422 = EDGE_CURVE ( 'NONE', #18257, #10863, #12197, .T. ) ;
#11423 = ORIENTED_EDGE ( 'NONE', *, *, #5992, .F. ) ;
#11424 = ORIENTED_EDGE ( 'NONE', *, *, #11976, .F. ) ;
#11425 = EDGE_CURVE ( 'NONE', #18025, #185, #18198, .T. ) ;
#11426 = CARTESIAN_POINT ( 'NONE',  ( -20.00369391078757886, -29.24501739517668142, 4.267572492083039570 ) ) ;
#11427 = AXIS2_PLACEMENT_3D ( 'NONE', #7249, #14693, #10075 ) ;
#11428 = EDGE_LOOP ( 'NONE', ( #8832, #5979, #13447, #10352, #16941, #7829, #13408, #13206, #10596, #17155 ) ) ;
#11429 = VECTOR ( 'NONE', #13391, 1000.000000000000227 ) ;
#11431 = EDGE_LOOP ( 'NONE', ( #1858, #7672, #3213, #11339 ) ) ;
#11430 = ORIENTED_EDGE ( 'NONE', *, *, #11659, .T. ) ;
#11432 = PRODUCT_DEFINITION_SHAPE ( 'NONE', 'NONE',  #19409 ) ;
#11433 = CARTESIAN_POINT ( 'NONE',  ( -17.31681416490115311, -26.07549068051209318, 2.294927507916959986 ) ) ;
#11434 = CARTESIAN_POINT ( 'NONE',  ( -22.04416526290807710, -25.71081734191525925, 34.23242750791695244 ) ) ;
#11435 = DIRECTION ( 'NONE',  ( -0.000000000000000000, -0.000000000000000000, -1.000000000000000000 ) ) ;
#11436 = CARTESIAN_POINT ( 'NONE',  ( 1.035533905932738197, 66.50000000000000000, 47.45000000218495018 ) ) ;
#11437 = LINE ( 'NONE', #2616, #14384 ) ;
#11438 = ORIENTED_EDGE ( 'NONE', *, *, #6601, .T. ) ;
#11439 = DIRECTION ( 'NONE',  ( 0.000000000000000000, -1.000000000000000000, 1.287488025362403787E-15 ) ) ;
#11440 = ORIENTED_EDGE ( 'NONE', *, *, #12384, .T. ) ;
#11441 = DIRECTION ( 'NONE',  ( -0.7071067811865437980, 0.5000000000000044409, -0.5000000000000008882 ) ) ;
#11442 = ORIENTED_EDGE ( 'NONE', *, *, #3875, .T. ) ;
#11443 = CARTESIAN_POINT ( 'NONE',  ( 0.2673660800788628111, 61.93276224060318214, 44.99999999999988631 ) ) ;
#11444 = FACE_BOUND ( 'NONE', #6478, .T. ) ;
#11445 = PLANE ( 'NONE',  #19076 ) ;
#11446 = CIRCLE ( 'NONE', #192, 2.500000000000000444 ) ;
#11447 = CARTESIAN_POINT ( 'NONE',  ( 2.066987300000002303, 63.14382582708705627, 45.90000000109247225 ) ) ;
#11448 = VECTOR ( 'NONE', #18597, 1000.000000000000000 ) ;
#11449 = DIRECTION ( 'NONE',  ( -1.000000000000000000, -0.000000000000000000, -0.000000000000000000 ) ) ;
#11450 = CARTESIAN_POINT ( 'NONE',  ( 1.035533905932739751, 61.50000000000000000, 49.44999999999999574 ) ) ;
#11451 = DIRECTION ( 'NONE',  ( -1.000000000000000000, 0.000000000000000000, 0.000000000000000000 ) ) ;
#11452 = EDGE_CURVE ( 'NONE', #9890, #8292, #4666, .T. ) ;
#11453 = VERTEX_POINT ( 'NONE', #4776 ) ;
#11454 = ORIENTED_EDGE ( 'NONE', *, *, #4372, .T. ) ;
#11455 = CARTESIAN_POINT ( 'NONE',  ( -18.35725562635144925, -17.85540867095761186, 9.076177507916954212 ) ) ;
#11456 = LINE ( 'NONE', #17448, #13340 ) ;
#11457 = ORIENTED_EDGE ( 'NONE', *, *, #12109, .T. ) ;
#11458 = CARTESIAN_POINT ( 'NONE',  ( -14.83517299489736985, -26.99999999999998579, 8.861322492083040459 ) ) ;
#11459 = AXIS2_PLACEMENT_3D ( 'NONE', #12746, #11268, #18741 ) ;
#11460 = CIRCLE ( 'NONE', #12415, 2.500000000000002220 ) ;
#11461 = PLANE ( 'NONE',  #1560 ) ;
#11462 = ORIENTED_EDGE ( 'NONE', *, *, #11635, .T. ) ;
#11463 = CARTESIAN_POINT ( 'NONE',  ( -16.64274437364858272, -21.48433729119797420, 37.29882249208304046 ) ) ;
#11464 = ORIENTED_EDGE ( 'NONE', *, *, #10420, .F. ) ;
#11465 = CARTESIAN_POINT ( 'NONE',  ( -41.00000000000000711, 110.0000000000000000, -37.50000000000000711 ) ) ;
#11466 = ORIENTED_EDGE ( 'NONE', *, *, #7218, .F. ) ;
#11467 = CARTESIAN_POINT ( 'NONE',  ( 14.99999999999998579, 52.00000000000000711, 20.99999999999997513 ) ) ;
#11468 = CARTESIAN_POINT ( 'NONE',  ( 7.500000000000005329, -38.00000000000000000, 12.50000000000000000 ) ) ;
#11469 = DIRECTION ( 'NONE',  ( 0.000000000000000000, 1.000000000000000000, 0.000000000000000000 ) ) ;
#11470 = LINE ( 'NONE', #17762, #979 ) ;
#11471 = COLOUR_RGB ( '', 0.40784314, 0.44705882, 0.49803922) ;
#11472 = EDGE_CURVE ( 'NONE', #15997, #18408, #6016, .T. ) ;
#11473 = CARTESIAN_POINT ( 'NONE',  ( -12.64274437364855252, -28.41254052147347053, 27.45117750791695954 ) ) ;
#11474 = FILL_AREA_STYLE_COLOUR ( '', #3574 ) ;
#11475 = EDGE_CURVE ( 'NONE', #13021, #18278, #11907, .T. ) ;
#11476 = CARTESIAN_POINT ( 'NONE',  ( -12.64274437364855252, -28.41254052147347053, 1.201177507916958431 ) ) ;
#11477 = CARTESIAN_POINT ( 'NONE',  ( -2.500000000000001776, 64.00000000000000000, 46.00000000000000000 ) ) ;
#11478 = ORIENTED_EDGE ( 'NONE', *, *, #13475, .F. ) ;
#11479 = CARTESIAN_POINT ( 'NONE',  ( -15.16482700510263371, -18.99999999999997868, 6.236322492083041347 ) ) ;
#11480 = CARTESIAN_POINT ( 'NONE',  ( -13.82508104294698192, -29.04416526290806644, 38.16992750791695244 ) ) ;
#11481 = CARTESIAN_POINT ( 'NONE',  ( 1.461580736456473906, 62.53841926354353120, 49.05000000109247082 ) ) ;
#11482 = CARTESIAN_POINT ( 'NONE',  ( -11.46040770435014977, -20.21908421996103655, 33.14257249208303335 ) ) ;
#11483 =( BOUNDED_CURVE ( )  B_SPLINE_CURVE ( 2, ( #8226, #13080, #14191, #6739, #6829, #11810, #13484, #19278, #8876 ),
 .UNSPECIFIED., .F., .F. ) 
 B_SPLINE_CURVE_WITH_KNOTS ( ( 3, 2, 2, 2, 3 ),
 ( 0.000000000000000000, 0.01785714285714280411, 0.03571428571428560822, 0.05357142857142841580, 0.07142857142857121644 ),
 .UNSPECIFIED. ) 
 CURVE ( )  GEOMETRIC_REPRESENTATION_ITEM ( )  RATIONAL_B_SPLINE_CURVE ( ( 1.000000000000000000, 0.9238795325112867385, 1.000000000000000000, 0.9238795325112867385, 1.000000000000000000, 0.9238795325112867385, 1.000000000000000000, 0.9238795325112876267, 0.9999999999999991118 ) ) 
 REPRESENTATION_ITEM ( '' )  );
#11484 = CARTESIAN_POINT ( 'NONE',  ( -25.00000000000000000, 53.00000000000000711, 8.000000000000000000 ) ) ;
#11485 = ORIENTED_EDGE ( 'NONE', *, *, #7988, .F. ) ;
#11486 = FACE_BOUND ( 'NONE', #1584, .T. ) ;
#11487 = CARTESIAN_POINT ( 'NONE',  ( -20.04416526290808065, -25.17491895705300209, 23.73242750791694888 ) ) ;
#11488 = DIRECTION ( 'NONE',  ( -0.000000000000000000, 1.000000000000000000, 0.000000000000000000 ) ) ;
#11489 = CARTESIAN_POINT ( 'NONE',  ( 41.00000000000000000, 47.00000000000000711, 18.00000000000000000 ) ) ;
#11490 = DIRECTION ( 'NONE',  ( -1.000000000000000000, 0.000000000000000000, 0.000000000000000000 ) ) ;
#11491 = CARTESIAN_POINT ( 'NONE',  ( 0.1499999999999973577, 0.000000000000000000, 0.000000000000000000 ) ) ;
#11492 = CARTESIAN_POINT ( 'NONE',  ( -0.8561741729129461742, 66.06698729999999387, 44.80000000109246372 ) ) ;
#11493 = CARTESIAN_POINT ( 'NONE',  ( 2.066987300000001415, 64.00000000000000000, 48.55000000109247082 ) ) ;
#11494 = EDGE_CURVE ( 'NONE', #3455, #13355, #15342, .T. ) ;
#11495 = CARTESIAN_POINT ( 'NONE',  ( 1.035533905932739751, 61.50000000000000000, 48.75000000218494023 ) ) ;
#11496 = CARTESIAN_POINT ( 'NONE',  ( 2.066987300000001415, 64.00000000000000000, 46.15000000109247225 ) ) ;
#11497 = LINE ( 'NONE', #17893, #1759 ) ;
#11498 = ORIENTED_EDGE ( 'NONE', *, *, #4238, .T. ) ;
#11499 = EDGE_CURVE ( 'NONE', #17265, #11522, #8194, .T. ) ;
#11500 = CARTESIAN_POINT ( 'NONE',  ( -0.8561741729129466183, 61.93301270000000613, 46.50000000109247367 ) ) ;
#11501 = CARTESIAN_POINT ( 'NONE',  ( -15.16482700510259640, -28.99999999999998224, 6.888677507916957765 ) ) ;
#11502 = DIRECTION ( 'NONE',  ( 0.000000000000000000, 0.000000000000000000, -1.000000000000000000 ) ) ;
#11503 = CARTESIAN_POINT ( 'NONE',  ( -20.24501739517669563, -18.99630608921239627, 37.08007249208304046 ) ) ;
#11504 = CARTESIAN_POINT ( 'NONE',  ( -1.265664690411616068E-16, 66.06698730000000808, 47.95000000109246940 ) ) ;
#11505 = CARTESIAN_POINT ( 'NONE',  ( -40.00000000000000711, 113.0000000000000000, -44.00000000000000000 ) ) ;
#11506 = DIRECTION ( 'NONE',  ( 0.000000000000000000, 0.7071067811865493491, -0.7071067811865457964 ) ) ;
#11507 = CARTESIAN_POINT ( 'NONE',  ( -2.066987300000001415, 64.00000000000000000, 47.15000000109247225 ) ) ;
#11508 = DIRECTION ( 'NONE',  ( 0.000000000000000000, 0.000000000000000000, -1.000000000000000000 ) ) ;
#11509 = VECTOR ( 'NONE', #6717, 1000.000000000000000 ) ;
#11510 = CARTESIAN_POINT ( 'NONE',  ( 2.500000000000000000, 1.768423874527823791, 1.020999999999998575 ) ) ;
#11511 = EDGE_CURVE ( 'NONE', #4095, #7547, #9456, .T. ) ;
#11512 = DIRECTION ( 'NONE',  ( 0.000000000000000000, 0.000000000000000000, 1.000000000000000000 ) ) ;
#11513 = EDGE_CURVE ( 'NONE', #7340, #12537, #1920, .T. ) ;
#11514 = EDGE_CURVE ( 'NONE', #2416, #717, #13200, .T. ) ;
#11515 = CARTESIAN_POINT ( 'NONE',  ( -2.499999999999992006, 62.96446609406726225, 44.55000000218494449 ) ) ;
#11516 = ORIENTED_EDGE ( 'NONE', *, *, #14751, .F. ) ;
#11517 = EDGE_LOOP ( 'NONE', ( #15554, #2518, #13031, #18565 ) ) ;
#11518 = CARTESIAN_POINT ( 'NONE',  ( -16.71081734191527346, -16.95583473709190159, 40.79492750791695244 ) ) ;
#11519 = CIRCLE ( 'NONE', #10001, 2.500000000000002220 ) ;
#11520 = ORIENTED_EDGE ( 'NONE', *, *, #15511, .T. ) ;
#11522 = VERTEX_POINT ( 'NONE', #3383 ) ;
#11521 = EDGE_LOOP ( 'NONE', ( #14788, #18484 ) ) ;
#11523 = CARTESIAN_POINT ( 'NONE',  ( -17.95583473709191580, -23.03132541760400898, 3.169927507916960874 ) ) ;
#11524 = CARTESIAN_POINT ( 'NONE',  ( -11.64274437364854187, -30.14459132904234195, 32.70117750791695244 ) ) ;
#11525 = VECTOR ( 'NONE', #19054, 1000.000000000000000 ) ;
#11526 = DIRECTION ( 'NONE',  ( 0.000000000000000000, 1.000000000000000000, 0.000000000000000000 ) ) ;
#11527 = CARTESIAN_POINT ( 'NONE',  ( 2.500000000000002220, 62.96446609406726935, 45.65000000218494591 ) ) ;
#11528 = FACE_OUTER_BOUND ( 'NONE', #85, .T. ) ;
#11529 = VERTEX_POINT ( 'NONE', #15443 ) ;
#11530 = CARTESIAN_POINT ( 'NONE',  ( 2.500000000000001776, 64.00000000000000000, 45.59999999999999432 ) ) ;
#11531 = VERTEX_POINT ( 'NONE', #9350 ) ;
#11532 = FACE_OUTER_BOUND ( 'NONE', #17132, .T. ) ;
#11533 = VERTEX_POINT ( 'NONE', #2009 ) ;
#11534 = DIRECTION ( 'NONE',  ( 1.000000000000000000, 0.000000000000000000, 0.000000000000000000 ) ) ;
#11535 = DIRECTION ( 'NONE',  ( 0.000000000000000000, 0.000000000000000000, -1.000000000000000000 ) ) ;
#11536 = LINE ( 'NONE', #17533, #5942 ) ;
#11537 = VECTOR ( 'NONE', #7211, 1000.000000000000000 ) ;
#11538 = CARTESIAN_POINT ( 'NONE',  ( -2.066987300000001415, 63.14382582708705627, 45.60000000109246088 ) ) ;
#11539 = EDGE_CURVE ( 'NONE', #11453, #14781, #17203, .T. ) ;
#11540 = DIRECTION ( 'NONE',  ( -1.000000000000000000, 0.000000000000000000, -0.000000000000000000 ) ) ;
#11541 = VECTOR ( 'NONE', #12845, 1000.000000000000000 ) ;
#11542 = LINE ( 'NONE', #10074, #2991 ) ;
#11543 = AXIS2_PLACEMENT_3D ( 'NONE', #5270, #2233, #6461 ) ;
#11544 = CARTESIAN_POINT ( 'NONE',  ( -1.040834085586084257E-14, 25.64142135623728080, 60.84386001800126564 ) ) ;
#11545 = ORIENTED_EDGE ( 'NONE', *, *, #14988, .F. ) ;
#11547 = ORIENTED_EDGE ( 'NONE', *, *, #6845, .F. ) ;
#11546 = EDGE_LOOP ( 'NONE', ( #12047, #8688, #18214, #15335 ) ) ;
#11548 = EDGE_CURVE ( 'NONE', #993, #11714, #7999, .T. ) ;
#11549 = CARTESIAN_POINT ( 'NONE',  ( -9.020235676060220698, -27.64274437364852588, 0.7636775079169565439 ) ) ;
#11550 = CARTESIAN_POINT ( 'NONE',  ( 37.49999999999999289, -6.000000000000000000, -25.00000000000001421 ) ) ;
#11551 = ORIENTED_EDGE ( 'NONE', *, *, #9760, .T. ) ;
#11552 = CARTESIAN_POINT ( 'NONE',  ( -11.95583473709190514, -24.63902057219072361, 7.767572492083043123 ) ) ;
#11553 = VECTOR ( 'NONE', #18573, 1000.000000000000114 ) ;
#11554 = CARTESIAN_POINT ( 'NONE',  ( -1.530808498934192803E-16, 66.50000000000000000, 45.00000000000000000 ) ) ;
#11555 = VERTEX_POINT ( 'NONE', #3769 ) ;
#11556 = CARTESIAN_POINT ( 'NONE',  ( -17.31681416490117087, -21.92450931948788551, 42.33007249208304756 ) ) ;
#11557 = VECTOR ( 'NONE', #2434, 1000.000000000000000 ) ;
#11558 = CARTESIAN_POINT ( 'NONE',  ( -32.50000000000000000, 52.00000000000000711, -32.35000000000000142 ) ) ;
#11559 = ORIENTED_EDGE ( 'NONE', *, *, #420, .T. ) ;
#11560 = CARTESIAN_POINT ( 'NONE',  ( -25.00000000000000711, 53.00000000000000711, -24.49999999999999645 ) ) ;
#11561 = ORIENTED_EDGE ( 'NONE', *, *, #18557, .T. ) ;
#11562 = ADVANCED_FACE ( 'NONE', ( #3673 ), #5059, .T. ) ;
#11563 = DIRECTION ( 'NONE',  ( 0.000000000000000000, 1.000000000000000000, 0.000000000000000000 ) ) ;
#11564 = CARTESIAN_POINT ( 'NONE',  ( -50.00000000000002132, 33.00000000000000000, 44.99999999999999289 ) ) ;
#11565 = CARTESIAN_POINT ( 'NONE',  ( -41.00000000000000711, 110.0000000000000000, -30.99999999999999645 ) ) ;
#11566 = VECTOR ( 'NONE', #6943, 1000.000000000000000 ) ;
#11567 = ITEM_DEFINED_TRANSFORMATION ( 'NONE', 'NONE', #17375,  #1791 ) ;
#11568 = LINE ( 'NONE', #16003, #17277 ) ;
#11569 = CARTESIAN_POINT ( 'NONE',  ( -16.50457296725820555, -28.95583473709189448, 22.85742750791695954 ) ) ;
#11570 = FACE_BOUND ( 'NONE', #19131, .T. ) ;
#11571 = ADVANCED_FACE ( 'NONE', ( #2201 ), #18395, .T. ) ;
#11572 = DIRECTION ( 'NONE',  ( 1.000000000000000000, 0.000000000000000000, 0.000000000000000000 ) ) ;
#11573 = VECTOR ( 'NONE', #18130, 1000.000000000000000 ) ;
#11574 = CARTESIAN_POINT ( 'NONE',  ( -15.20357423236093375, -43.78611686177728046, 3.000000000000000000 ) ) ;
#11575 = EDGE_LOOP ( 'NONE', ( #17172, #5410, #5117, #14808 ) ) ;
#11576 = PRODUCT_DEFINITION_CONTEXT ( 'detailed design', #6073, 'design' ) ;
#11577 = CARTESIAN_POINT ( 'NONE',  ( -19.95583473709190514, -25.50457296725822687, 9.955072492083036906 ) ) ;
#11578 = CARTESIAN_POINT ( 'NONE',  ( -17.04047135212043784, -30.95583473709190159, 1.857427507916956211 ) ) ;
#11579 = VECTOR ( 'NONE', #18663, 1000.000000000000000 ) ;
#11580 = CARTESIAN_POINT ( 'NONE',  ( 2.066987300000001859, 64.85617417291294373, 49.20000000109247651 ) ) ;
#11581 = CARTESIAN_POINT ( 'NONE',  ( -14.36097942780925685, -20.95583473709189093, 11.70507249208304223 ) ) ;
#11582 = DIRECTION ( 'NONE',  ( -0.7071067811865562325, -0.4999999999999955036, 0.4999999999999924505 ) ) ;
#11583 = ORIENTED_EDGE ( 'NONE', *, *, #15603, .T. ) ;
#11584 = AXIS2_PLACEMENT_3D ( 'NONE', #40, #10413, #9151 ) ;
#11585 = CARTESIAN_POINT ( 'NONE',  ( 2.500000000000004441, 62.96446609406726225, 46.45000000218494307 ) ) ;
#11586 = CARTESIAN_POINT ( 'NONE',  ( -19.24771351637089367, -21.35725562635142438, 29.63867750791695599 ) ) ;
#11587 = CARTESIAN_POINT ( 'NONE',  ( -0.9999999999999945599, -36.00000000000000711, 4.500000000000000888 ) ) ;
#11588 = VECTOR ( 'NONE', #4116, 1000.000000000000000 ) ;
#11589 = LINE ( 'NONE', #4163, #6840 ) ;
#11590 = CARTESIAN_POINT ( 'NONE',  ( -9.999999999999994671, -23.83517299489734143, 33.79882249208304046 ) ) ;
#11591 = CARTESIAN_POINT ( 'NONE',  ( 4.592425496802577917E-16, 61.50000000000000000, 46.99999999999999289 ) ) ;
#11592 = DIRECTION ( 'NONE',  ( 0.7071067811865535679, 0.4999999999999971134, -0.4999999999999944489 ) ) ;
#11593 = VECTOR ( 'NONE', #3908, 1000.000000000000000 ) ;
#11594 = CARTESIAN_POINT ( 'NONE',  ( -3.065533689247737392, -46.96461745799954457, 3.000000000000000000 ) ) ;
#11595 = CARTESIAN_POINT ( 'NONE',  ( 1.461580736456473906, 62.53841926354353120, 45.25000000109247367 ) ) ;
#11596 = LINE ( 'NONE', #13464, #18373 ) ;
#11597 = VECTOR ( 'NONE', #14330, 1000.000000000000000 ) ;
#11598 = VERTEX_POINT ( 'NONE', #17018 ) ;
#11599 = CIRCLE ( 'NONE', #7877, 2.500000000000001776 ) ;
#11600 = FACE_OUTER_BOUND ( 'NONE', #15906, .T. ) ;
#11601 = CARTESIAN_POINT ( 'NONE',  ( -20.04416526290808065, -25.17491895705300209, 7.982427507916958653 ) ) ;
#11602 = DIRECTION ( 'NONE',  ( 1.000000000000000000, 0.000000000000000000, -0.000000000000000000 ) ) ;
#11603 = CARTESIAN_POINT ( 'NONE',  ( -21.99999999999999289, -24.16482700510262305, 31.17382249208304046 ) ) ;
#11604 = AXIS2_PLACEMENT_3D ( 'NONE', #17320, #12893, #18893 ) ;
#11605 = CARTESIAN_POINT ( 'NONE',  ( 1.461580736456473684, 65.46158073645646880, 48.65000000109247225 ) ) ;
#11606 = CARTESIAN_POINT ( 'NONE',  ( -16.35725562635142794, -21.31951028609535470, 35.32617750791695244 ) ) ;
#11607 = CARTESIAN_POINT ( 'NONE',  ( -10.04416526290807710, -25.50457296725819489, 0.5449275079169580982 ) ) ;
#11608 = FACE_OUTER_BOUND ( 'NONE', #1030, .T. ) ;
#11609 = AXIS2_PLACEMENT_3D ( 'NONE', #1536, #17607, #3093 ) ;
#11610 = FACE_OUTER_BOUND ( 'NONE', #5636, .T. ) ;
#11611 = DIRECTION ( 'NONE',  ( -1.000000000000000000, 0.000000000000000000, -0.000000000000000000 ) ) ;
#11612 = ADVANCED_FACE ( 'NONE', ( #11017 ), #13769, .T. ) ;
#11613 = EDGE_CURVE ( 'NONE', #3909, #13439, #3829, .T. ) ;
#11614 = VECTOR ( 'NONE', #14241, 1000.000000000000114 ) ;
#11615 = CARTESIAN_POINT ( 'NONE',  ( -1.035533905932738863, 61.50000000000000000, 47.74999999999999289 ) ) ;
#11616 = CARTESIAN_POINT ( 'NONE',  ( -1.265664690411616068E-16, 66.06698730000000808, 47.15000000109247225 ) ) ;
#11617 = LINE ( 'NONE', #4084, #10343 ) ;
#11618 = ADVANCED_FACE ( 'NONE', ( #5151 ), #9643, .T. ) ;
#11619 = DIRECTION ( 'NONE',  ( -0.000000000000000000, -0.000000000000000000, 1.000000000000000000 ) ) ;
#11620 = ORIENTED_EDGE ( 'NONE', *, *, #13067, .F. ) ;
#11621 = VERTEX_POINT ( 'NONE', #8094 ) ;
#11622 = CARTESIAN_POINT ( 'NONE',  ( -21.99999999999999289, -24.16482700510262305, 4.923822492083038682 ) ) ;
#11623 = EDGE_CURVE ( 'NONE', #2609, #10285, #635, .T. ) ;
#11624 = ORIENTED_EDGE ( 'NONE', *, *, #3524, .T. ) ;
#11625 = CARTESIAN_POINT ( 'NONE',  ( -2.500000000000001776, 64.00000000000000000, 49.19999999999999574 ) ) ;
#11627 = ORIENTED_EDGE ( 'NONE', *, *, #5467, .T. ) ;
#11626 = ORIENTED_EDGE ( 'NONE', *, *, #10329, .T. ) ;
#11628 = CARTESIAN_POINT ( 'NONE',  ( -17.95583473709190869, -24.96867458239598037, 41.45507249208304046 ) ) ;
#11629 = CARTESIAN_POINT ( 'NONE',  ( -8.044165262908075320, -26.04047135212042718, 37.29492750791695954 ) ) ;
#11630 = AXIS2_PLACEMENT_3D ( 'NONE', #11778, #17770, #10302 ) ;
#11631 = DIRECTION ( 'NONE',  ( -0.000000000000000000, -0.000000000000000000, -1.000000000000000000 ) ) ;
#11632 = CARTESIAN_POINT ( 'NONE',  ( -2.500000000000001776, 65.03553390593273775, 45.25000000218494733 ) ) ;
#11633 = DIRECTION ( 'NONE',  ( 0.000000000000000000, -1.000000000000000000, 0.000000000000000000 ) ) ;
#11634 = VERTEX_POINT ( 'NONE', #6625 ) ;
#11635 = EDGE_CURVE ( 'NONE', #3717, #4896, #18584, .T. ) ;
#11636 = CARTESIAN_POINT ( 'NONE',  ( -4.101219330882018177, 26.84264068711928530, 59.64264068711926825 ) ) ;
#11637 = EDGE_LOOP ( 'NONE', ( #5133, #16812, #10141, #1386 ) ) ;
#11638 = ORIENTED_EDGE ( 'NONE', *, *, #2398, .T. ) ;
#11639 = PLANE ( 'NONE',  #15100 ) ;
#11640 = FACE_OUTER_BOUND ( 'NONE', #6844, .T. ) ;
#11641 = FACE_OUTER_BOUND ( 'NONE', #8900, .T. ) ;
#11642 = CARTESIAN_POINT ( 'NONE',  ( -1.461580736456473906, 65.46158073645646880, 49.65000000109246514 ) ) ;
#11643 = ADVANCED_FACE ( 'NONE', ( #349 ), #12680, .T. ) ;
#11644 = DIRECTION ( 'NONE',  ( 0.000000000000000000, 0.000000000000000000, -1.000000000000000000 ) ) ;
#11645 = DIRECTION ( 'NONE',  ( 0.000000000000000000, 0.000000000000000000, -1.000000000000000000 ) ) ;
#11646 = FACE_OUTER_BOUND ( 'NONE', #14498, .T. ) ;
#11647 = ORIENTED_EDGE ( 'NONE', *, *, #3941, .F. ) ;
#11649 = EDGE_LOOP ( 'NONE', ( #18533, #14102, #15262, #1173 ) ) ;
#11648 = ORIENTED_EDGE ( 'NONE', *, *, #8254, .F. ) ;
#11650 = CARTESIAN_POINT ( 'NONE',  ( -7.955834737091916686, -22.28918265808470522, 0.1074275079169565300 ) ) ;
#11651 = DIRECTION ( 'NONE',  ( -0.000000000000000000, -1.000000000000000000, -0.000000000000000000 ) ) ;
#11652 = VERTEX_POINT ( 'NONE', #17583 ) ;
#11653 = VERTEX_POINT ( 'NONE', #14634 ) ;
#11654 = CARTESIAN_POINT ( 'NONE',  ( -17.31681416490117087, -21.92450931948788551, 5.580072492083043123 ) ) ;
#11655 = ADVANCED_FACE ( 'NONE', ( #12960 ), #5433, .T. ) ;
#11656 = EDGE_CURVE ( 'NONE', #9185, #17434, #19050, .T. ) ;
#11657 = CARTESIAN_POINT ( 'NONE',  ( -1.530808498934192803E-16, 66.50000000000000000, 45.00000000000000000 ) ) ;
#11658 = ORIENTED_EDGE ( 'NONE', *, *, #5288, .T. ) ;
#11659 = EDGE_CURVE ( 'NONE', #11681, #4215, #6754, .T. ) ;
#11660 = CARTESIAN_POINT ( 'NONE',  ( -15.16482700510260706, -26.99999999999998579, 1.638677507916960208 ) ) ;
#11661 = CARTESIAN_POINT ( 'NONE',  ( -2.500000000000001776, 64.00000000000000000, 44.50000000218494733 ) ) ;
#11662 = ORIENTED_EDGE ( 'NONE', *, *, #8398, .F. ) ;
#11663 = FACE_OUTER_BOUND ( 'NONE', #17628, .T. ) ;
#11664 = ORIENTED_EDGE ( 'NONE', *, *, #4011, .T. ) ;
#11665 = CARTESIAN_POINT ( 'NONE',  ( -44.99999999999998579, 0.000000000000000000, -53.40000000000000568 ) ) ;
#11666 = ADVANCED_FACE ( 'NONE', ( #19154, #3861, #17474, #9918, #5724, #11486, #15914 ), #8466, .T. ) ;
#11667 = DIRECTION ( 'NONE',  ( 0.000000000000000000, -0.000000000000000000, -1.000000000000000000 ) ) ;
#11668 = DIRECTION ( 'NONE',  ( 0.7071067811865535679, 0.4999999999999971134, -0.4999999999999944489 ) ) ;
#11669 = LINE ( 'NONE', #13238, #8813 ) ;
#11670 = CARTESIAN_POINT ( 'NONE',  ( -19.24771351637089367, -21.35725562635142438, 24.38867750791695954 ) ) ;
#11671 = DIRECTION ( 'NONE',  ( -0.1648270051026180794, 0.000000000000000000, 0.9863224920830415687 ) ) ;
#11672 = FACE_OUTER_BOUND ( 'NONE', #15273, .T. ) ;
#11673 = CARTESIAN_POINT ( 'NONE',  ( -25.00000000000000000, 53.00000000000000711, -32.00000000000000000 ) ) ;
#11674 = VERTEX_POINT ( 'NONE', #15734 ) ;
#11675 = EDGE_CURVE ( 'NONE', #2269, #9366, #14442, .T. ) ;
#11676 = CARTESIAN_POINT ( 'NONE',  ( -20.24501739517669563, -18.99630608921239627, 42.33007249208303335 ) ) ;
#11677 = CARTESIAN_POINT ( 'NONE',  ( -17.04047135212043784, -30.95583473709190159, 7.107427507916957765 ) ) ;
#11678 = CARTESIAN_POINT ( 'NONE',  ( 0.1249999999999895917, 25.64142146683625612, 60.84290755733282197 ) ) ;
#11679 = CARTESIAN_POINT ( 'NONE',  ( -19.95583473709190514, -25.50457296725822687, 41.45507249208304046 ) ) ;
#11680 = DIRECTION ( 'NONE',  ( 0.000000000000000000, -0.7071067811865495711, 0.7071067811865454633 ) ) ;
#11681 = VERTEX_POINT ( 'NONE', #11300 ) ;
#11682 = LINE ( 'NONE', #7087, #17213 ) ;
#11683 = CARTESIAN_POINT ( 'NONE',  ( -16.50457296725820555, -28.95583473709189448, 38.60742750791694533 ) ) ;
#11684 = LINE ( 'NONE', #5528, #15488 ) ;
#11685 = CARTESIAN_POINT ( 'NONE',  ( -1.035533905932738641, 66.50000000000000000, 45.15000000218493881 ) ) ;
#11686 = CARTESIAN_POINT ( 'NONE',  ( -1.040834085586084257E-14, 25.49999999999998934, 52.50000000000000000 ) ) ;
#11687 = CARTESIAN_POINT ( 'NONE',  ( -16.50457296725825174, -19.04416526290807354, 37.51757249208304046 ) ) ;
#11688 = PRODUCT_DEFINITION ( 'UNKNOWN', '', #8927, #10795 ) ;
#11689 =( REPRESENTATION_RELATIONSHIP ('NONE','NONE', #7912, #13906 ) REPRESENTATION_RELATIONSHIP_WITH_TRANSFORMATION ( #11567 )SHAPE_REPRESENTATION_RELATIONSHIP( ) );
#11690 = CARTESIAN_POINT ( 'NONE',  ( -1.035533905932738863, 61.50000000000000000, 46.14999999999999858 ) ) ;
#11691 = CARTESIAN_POINT ( 'NONE',  ( -2.066987300000000971, 63.14382582708704916, 46.60000000109246798 ) ) ;
#11692 = FACE_BOUND ( 'NONE', #18653, .T. ) ;
#11693 = CARTESIAN_POINT ( 'NONE',  ( -1.035533905932738863, 61.50000000000000000, 46.95000000000000995 ) ) ;
#11694 = LINE ( 'NONE', #17686, #5213 ) ;
#11695 = EDGE_CURVE ( 'NONE', #3613, #5230, #11682, .T. ) ;
#11696 = ORIENTED_EDGE ( 'NONE', *, *, #4730, .F. ) ;
#11697 = LINE ( 'NONE', #17990, #9065 ) ;
#11698 = VECTOR ( 'NONE', #12670, 1000.000000000000000 ) ;
#11699 = CARTESIAN_POINT ( 'NONE',  ( -12.35725562635143682, -19.75228648362908501, 4.701177507916957765 ) ) ;
#11700 = CARTESIAN_POINT ( 'NONE',  ( -2.500000000000001776, 65.03553390593273775, 48.45000000218495018 ) ) ;
#11701 = CARTESIAN_POINT ( 'NONE',  ( -18.78091578003892081, -20.46040770435013556, 5.580072492083041347 ) ) ;
#11702 = CARTESIAN_POINT ( 'NONE',  ( 1.461580736456473684, 65.46158073645646880, 49.45000000109246940 ) ) ;
#11703 = CARTESIAN_POINT ( 'NONE',  ( -17.31681416490115311, -26.07549068051209318, 39.04492750791695954 ) ) ;
#11704 = CARTESIAN_POINT ( 'NONE',  ( -19.24771351637089367, -21.35725562635142438, 8.638677507916957765 ) ) ;
#11705 = CARTESIAN_POINT ( 'NONE',  ( 12.99999999999999822, 2.516649172247811061E-16, -2.055000000000000160 ) ) ;
#11706 = CARTESIAN_POINT ( 'NONE',  ( 0.000000000000000000, 2.357898499370431722, -2.818925648462311528E-15 ) ) ;
#11707 = FACE_BOUND ( 'NONE', #18806, .T. ) ;
#11708 = PRESENTATION_LAYER_ASSIGNMENT (  '', '', ( #13598 ) ) ;
#11709 = FACE_BOUND ( 'NONE', #2834, .T. ) ;
#11710 = VECTOR ( 'NONE', #14737, 1000.000000000000000 ) ;
#11711 = CARTESIAN_POINT ( 'NONE',  ( 0.8561741729129460632, 66.06698730000000808, 47.10000000109246798 ) ) ;
#11712 = CARTESIAN_POINT ( 'NONE',  ( 20.00000000000000355, 0.000000000000000000, 1.500000000000000000 ) ) ;
#11713 = CARTESIAN_POINT ( 'NONE',  ( -2.750000000000020872, 118.0000000000000000, 37.49999999999997158 ) ) ;
#11714 = VERTEX_POINT ( 'NONE', #17298 ) ;
#11715 = ORIENTED_EDGE ( 'NONE', *, *, #14861, .T. ) ;
#11716 = CARTESIAN_POINT ( 'NONE',  ( -18.64274437364853654, -29.97976432393976509, 38.82617750791695244 ) ) ;
#11717 =( NAMED_UNIT ( * ) PLANE_ANGLE_UNIT ( ) SI_UNIT ( $, .RADIAN. ) );
#11718 = DIRECTION ( 'NONE',  ( 0.000000000000000000, 0.000000000000000000, 1.000000000000000000 ) ) ;
#11720 = ORIENTED_EDGE ( 'NONE', *, *, #12958, .F. ) ;
#11719 = ORIENTED_EDGE ( 'NONE', *, *, #11793, .F. ) ;
#11721 = CARTESIAN_POINT ( 'NONE',  ( -16.35725562635142794, -21.31951028609535470, 3.826177507916959986 ) ) ;
#11722 = CARTESIAN_POINT ( 'NONE',  ( -21.95583473709189803, -26.04047135212049469, 9.955072492083038682 ) ) ;
#11723 = VECTOR ( 'NONE', #16000, 1000.000000000000000 ) ;
#11724 = DIRECTION ( 'NONE',  ( 0.000000000000000000, 0.000000000000000000, -1.000000000000000000 ) ) ;
#11725 = CARTESIAN_POINT ( 'NONE',  ( 1.035533905932739751, 61.50000000000000000, 45.55000000218493739 ) ) ;
#11726 = EDGE_LOOP ( 'NONE', ( #10109, #8666, #14666, #5870 ) ) ;
#11727 = EDGE_LOOP ( 'NONE', ( #14526, #168, #2380, #18911, #11105 ) ) ;
#11728 = CARTESIAN_POINT ( 'NONE',  ( 2.500000000000007105, 62.96446609406726225, 46.34999999999998721 ) ) ;
#11729 = ORIENTED_EDGE ( 'NONE', *, *, #18972, .T. ) ;
#11730 = ORIENTED_EDGE ( 'NONE', *, *, #5052, .F. ) ;
#11731 = CARTESIAN_POINT ( 'NONE',  ( 3.999999999999998224, 67.00000000000000000, 34.99999999999999289 ) ) ;
#11732 = DIRECTION ( 'NONE',  ( 0.000000000000000000, -0.6139406135149195753, 0.7893522173763268812 ) ) ;
#11733 = CARTESIAN_POINT ( 'NONE',  ( -40.00000000000000711, 113.0000000000000000, 27.50000000000000000 ) ) ;
#11734 = CARTESIAN_POINT ( 'NONE',  ( -1.461580736456473906, 65.46158073645646880, 46.45000000109246940 ) ) ;
#11735 = CARTESIAN_POINT ( 'NONE',  ( 2.750000000000009770, 38.00000000000000000, -42.68883962248118991 ) ) ;
#11736 = AXIS2_PLACEMENT_3D ( 'NONE', #14924, #16589, #1497 ) ;
#11737 = CARTESIAN_POINT ( 'NONE',  ( -1.035533905932738863, 61.50000000000000000, 47.05000000218494449 ) ) ;
#11738 = VECTOR ( 'NONE', #6060, 1000.000000000000000 ) ;
#11739 = DIRECTION ( 'NONE',  ( -1.000000000000000000, 0.000000000000000000, -0.000000000000000000 ) ) ;
#11740 = ORIENTED_EDGE ( 'NONE', *, *, #2352, .F. ) ;
#11742 = VERTEX_POINT ( 'NONE', #6991 ) ;
#11741 = ORIENTED_EDGE ( 'NONE', *, *, #3846, .F. ) ;
#11743 = CARTESIAN_POINT ( 'NONE',  ( -16.71081734191527346, -16.95583473709190159, 4.044927507916956877 ) ) ;
#11744 = DIRECTION ( 'NONE',  ( 0.000000000000000000, 0.000000000000000000, 1.000000000000000000 ) ) ;
#11745 = ORIENTED_EDGE ( 'NONE', *, *, #124, .F. ) ;
#11746 = ORIENTED_EDGE ( 'NONE', *, *, #11190, .F. ) ;
#11747 = CARTESIAN_POINT ( 'NONE',  ( -9.955834737091903364, -25.17491895705294880, 39.26757249208304046 ) ) ;
#11748 = EDGE_CURVE ( 'NONE', #11044, #7973, #10110, .T. ) ;
#11749 = DIRECTION ( 'NONE',  ( 1.000000000000000000, 2.168404344971008868E-16, 0.000000000000000000 ) ) ;
#11750 = PLANE ( 'NONE',  #5635 ) ;
#11751 = VERTEX_POINT ( 'NONE', #8653 ) ;
#11752 = CARTESIAN_POINT ( 'NONE',  ( -11.95583473709191047, -23.36097942780921954, 0.1074275079169599995 ) ) ;
#11753 = AXIS2_PLACEMENT_3D ( 'NONE', #3567, #14053, #3206 ) ;
#11754 = DIRECTION ( 'NONE',  ( 0.1648270051026190508, 0.000000000000000000, -0.9863224920830413467 ) ) ;
#11755 = ORIENTED_EDGE ( 'NONE', *, *, #9984, .F. ) ;
#11756 = AXIS2_PLACEMENT_3D ( 'NONE', #2977, #16213, #7100 ) ;
#11757 = LINE ( 'NONE', #17955, #4709 ) ;
#11758 = PRODUCT ( 'electro magnet', 'electro magnet', '', ( #5801 ) ) ;
#11759 = EDGE_LOOP ( 'NONE', ( #6052, #6664, #13326, #7265 ) ) ;
#11760 = PLANE ( 'NONE',  #19 ) ;
#11761 = CARTESIAN_POINT ( 'NONE',  ( 0.000000000000000000, 64.00000000000000000, 49.99999999999999289 ) ) ;
#11762 = CARTESIAN_POINT ( 'NONE',  ( 49.99999999999998579, 0.000000000000000000, 59.99999999999997868 ) ) ;
#11763 = SHAPE_DEFINITION_REPRESENTATION ( #5829, #15417 ) ;
#11764 = CARTESIAN_POINT ( 'NONE',  ( -41.00000000000000711, 53.00000000000000711, 1.500000000000001332 ) ) ;
#11765 = EDGE_CURVE ( 'NONE', #14478, #7973, #10016, .T. ) ;
#11766 = CARTESIAN_POINT ( 'NONE',  ( -9.955834737091912245, -22.82508104294696594, 21.10742750791695599 ) ) ;
#11767 = EDGE_CURVE ( 'NONE', #9777, #11949, #5525, .T. ) ;
#11768 = CARTESIAN_POINT ( 'NONE',  ( -24.00000000000000711, 110.0000000000000000, 14.50000000000000000 ) ) ;
#11769 = EDGE_CURVE ( 'NONE', #4322, #8618, #8280, .T. ) ;
#11770 = CARTESIAN_POINT ( 'NONE',  ( -10.58745947852649927, -21.64274437364853654, 5.138677507916957765 ) ) ;
#11771 = VECTOR ( 'NONE', #2759, 1000.000000000000000 ) ;
#11773 = FACE_OUTER_BOUND ( 'NONE', #16775, .T. ) ;
#11772 = ADVANCED_BREP_SHAPE_REPRESENTATION ( '', ( #4051, #1791 ), #15487 ) ;
#11774 = ORIENTED_EDGE ( 'NONE', *, *, #2404, .T. ) ;
#11775 = AXIS2_PLACEMENT_3D ( 'NONE', #15310, #15419, #7873 ) ;
#11776 = CARTESIAN_POINT ( 'NONE',  ( -14.83517299489735741, -28.99999999999998224, 3.611322492083041347 ) ) ;
#11777 = CARTESIAN_POINT ( 'NONE',  ( -20.00369391078762860, -18.75498260482333279, 8.857427507916955989 ) ) ;
#11778 = CARTESIAN_POINT ( 'NONE',  ( 4.999999999999997335, 0.000000000000000000, 0.000000000000000000 ) ) ;
#11779 = CARTESIAN_POINT ( 'NONE',  ( -11.99999999999999289, -23.83517299489735564, 7.548822492083043123 ) ) ;
#11780 = LINE ( 'NONE', #4347, #18501 ) ;
#11781 = VERTEX_POINT ( 'NONE', #2386 ) ;
#11782 = DIRECTION ( 'NONE',  ( -0.000000000000000000, -1.000000000000000000, -0.000000000000000000 ) ) ;
#11783 = ORIENTED_EDGE ( 'NONE', *, *, #6055, .F. ) ;
#11784 = LINE ( 'NONE', #8654, #6249 ) ;
#11785 = CARTESIAN_POINT ( 'NONE',  ( -41.00000000000000711, 53.00000000000000711, 21.00000000000000000 ) ) ;
#11786 = AXIS2_PLACEMENT_3D ( 'NONE', #14699, #5782, #11843 ) ;
#11787 = DIRECTION ( 'NONE',  ( 1.000000000000000000, -0.000000000000000000, -0.000000000000000000 ) ) ;
#11788 = DIRECTION ( 'NONE',  ( 0.000000000000000000, -1.000000000000000000, 0.000000000000000000 ) ) ;
#11789 = LINE ( 'NONE', #17780, #8465 ) ;
#11790 = VECTOR ( 'NONE', #17307, 1000.000000000000000 ) ;
#11791 = CARTESIAN_POINT ( 'NONE',  ( -1.767766952966369765, 62.23223304703363112, 46.89999999999999858 ) ) ;
#11792 = CARTESIAN_POINT ( 'NONE',  ( -2.066987300000001415, 64.85617417291294373, 46.50000000109246656 ) ) ;
#11793 = EDGE_CURVE ( 'NONE', #14672, #18913, #14342, .T. ) ;
#11794 = CARTESIAN_POINT ( 'NONE',  ( -4.012830983233618198, 32.52836399182267257, 53.60336399182263989 ) ) ;
#11795 = CARTESIAN_POINT ( 'NONE',  ( 1.767766952966370653, 62.23223304703363112, 47.09999999999999432 ) ) ;
#11796 = LINE ( 'NONE', #19261, #3330 ) ;
#11797 = ORIENTED_EDGE ( 'NONE', *, *, #6845, .T. ) ;
#11798 =( NAMED_UNIT ( * ) SI_UNIT ( $, .STERADIAN. ) SOLID_ANGLE_UNIT ( ) );
#11799 = CARTESIAN_POINT ( 'NONE',  ( -19.95583473709191580, -22.49542703274176603, 3.169927507916957321 ) ) ;
#11800 = CARTESIAN_POINT ( 'NONE',  ( -13.49542703274178379, -19.04416526290806289, 9.732427507916959541 ) ) ;
#11801 = CARTESIAN_POINT ( 'NONE',  ( 4.592425496802577917E-16, 61.50000000000000000, 48.70000000218494307 ) ) ;
#11802 = CARTESIAN_POINT ( 'NONE',  ( -19.24771351637086880, -26.64274437364857206, 4.486322492083041347 ) ) ;
#11803 = CARTESIAN_POINT ( 'NONE',  ( -41.99999999999997868, 6.000000000000005329, 51.99999999999997868 ) ) ;
#11804 = CARTESIAN_POINT ( 'NONE',  ( -11.46040770435012668, -27.78091578003887463, 6.232427507916956877 ) ) ;
#11805 = CARTESIAN_POINT ( 'NONE',  ( -10.75228648362910100, -26.64274437364854009, 0.7636775079169582092 ) ) ;
#11806 = DIRECTION ( 'NONE',  ( 0.000000000000000000, -1.000000000000000000, -0.000000000000000000 ) ) ;
#11807 = EDGE_CURVE ( 'NONE', #996, #17064, #4060, .T. ) ;
#11808 = DIRECTION ( 'NONE',  ( 1.000000000000000000, -0.000000000000000000, -0.000000000000000000 ) ) ;
#11809 = CARTESIAN_POINT ( 'NONE',  ( 46.99999999999998579, 118.0000000000000142, 56.99999999999997158 ) ) ;
#11810 = CARTESIAN_POINT ( 'NONE',  ( 1.035533905932738197, 66.50000000000000000, 49.74999999999998579 ) ) ;
#11811 = CARTESIAN_POINT ( 'NONE',  ( -40.00000000000000711, 110.0000000000000000, 30.00000000000000000 ) ) ;
#11812 = CARTESIAN_POINT ( 'NONE',  ( 2.500000000000001776, 64.00000000000000000, 44.90000000218493881 ) ) ;
#11813 = LINE ( 'NONE', #13280, #5512 ) ;
#11814 = VERTEX_POINT ( 'NONE', #12870 ) ;
#11815 = ADVANCED_FACE ( 'NONE', ( #12770 ), #231, .T. ) ;
#11816 = ORIENTED_EDGE ( 'NONE', *, *, #8201, .T. ) ;
#11817 = CARTESIAN_POINT ( 'NONE',  ( -8.855408670957602979, -27.35725562635137820, 18.48632249208304046 ) ) ;
#11818 = DIRECTION ( 'NONE',  ( 0.000000000000000000, -1.000000000000000000, 0.000000000000000000 ) ) ;
#11820 = ORIENTED_EDGE ( 'NONE', *, *, #1632, .T. ) ;
#11819 = ORIENTED_EDGE ( 'NONE', *, *, #11539, .F. ) ;
#11821 = CARTESIAN_POINT ( 'NONE',  ( -17.07549068051210739, -21.68318583509881847, 14.10742750791695954 ) ) ;
#11822 = CARTESIAN_POINT ( 'NONE',  ( -8.528048594804062077, -45.28611686177728046, 3.000000000000000000 ) ) ;
#11823 = CARTESIAN_POINT ( 'NONE',  ( -7.955834737091903364, -25.71081734191518464, 2.517572492083039126 ) ) ;
#11824 = PLANE ( 'NONE',  #6330 ) ;
#11825 = CARTESIAN_POINT ( 'NONE',  ( 2.066987300000001415, 64.00000000000000000, 49.15000000109247225 ) ) ;
#11826 = VERTEX_POINT ( 'NONE', #8850 ) ;
#11827 = ORIENTED_EDGE ( 'NONE', *, *, #17785, .F. ) ;
#11828 = VECTOR ( 'NONE', #8973, 1000.000000000000000 ) ;
#11829 = CARTESIAN_POINT ( 'NONE',  ( -41.00000000000000711, 53.00000000000000711, -37.50000000000000711 ) ) ;
#11830 = LINE ( 'NONE', #1359, #11331 ) ;
#11831 = ORIENTED_EDGE ( 'NONE', *, *, #217, .F. ) ;
#11832 = EDGE_CURVE ( 'NONE', #18667, #2908, #6215, .T. ) ;
#11833 = DIRECTION ( 'NONE',  ( 6.672013369141567928E-17, 0.000000000000000000, -1.000000000000000000 ) ) ;
#11834 = DIRECTION ( 'NONE',  ( -1.000000000000000000, -2.312964634635742957E-16, 0.000000000000000000 ) ) ;
#11835 = CARTESIAN_POINT ( 'NONE',  ( 1.461580736456473684, 65.46158073645646880, 48.65000000109247225 ) ) ;
#11836 = DIRECTION ( 'NONE',  ( 0.000000000000000000, -1.000000000000000000, 1.026972870230479989E-15 ) ) ;
#11837 = DIRECTION ( 'NONE',  ( 0.000000000000000000, -0.000000000000000000, 1.000000000000000000 ) ) ;
#11838 = EDGE_LOOP ( 'NONE', ( #7451, #1574, #3657, #4303 ) ) ;
#11840 = ORIENTED_EDGE ( 'NONE', *, *, #5697, .F. ) ;
#11839 = VERTEX_POINT ( 'NONE', #17879 ) ;
#11841 = CARTESIAN_POINT ( 'NONE',  ( -7.955834737091916686, -22.28918265808470522, 21.10742750791695954 ) ) ;
#11842 = AXIS2_PLACEMENT_3D ( 'NONE', #10313, #11888, #14740 ) ;
#11843 = DIRECTION ( 'NONE',  ( 0.000000000000000000, 0.000000000000000000, -1.000000000000000000 ) ) ;
#11844 = VERTEX_POINT ( 'NONE', #7476 ) ;
#11845 = ORIENTED_EDGE ( 'NONE', *, *, #12916, .F. ) ;
#11846 = CARTESIAN_POINT ( 'NONE',  ( -11.99999999999999289, -23.83517299489735564, 2.298822492083042235 ) ) ;
#11847 = CARTESIAN_POINT ( 'NONE',  ( 50.00000000000000000, 118.0000000000000142, -60.00000000000000000 ) ) ;
#11848 = PLANE ( 'NONE',  #13765 ) ;
#11849 = ORIENTED_EDGE ( 'NONE', *, *, #9023, .F. ) ;
#11850 = CARTESIAN_POINT ( 'NONE',  ( -15.96867458239597326, -26.95583473709190159, 7.107427507916960430 ) ) ;
#11851 = VECTOR ( 'NONE', #10070, 1000.000000000000000 ) ;
#11852 = DIRECTION ( 'NONE',  ( 0.000000000000000000, 0.000000000000000000, 1.000000000000000000 ) ) ;
#11853 = ORIENTED_EDGE ( 'NONE', *, *, #5674, .T. ) ;
#11854 = DIRECTION ( 'NONE',  ( -5.782411586589357392E-17, 0.000000000000000000, -1.000000000000000000 ) ) ;
#11855 = ORIENTED_EDGE ( 'NONE', *, *, #18746, .F. ) ;
#11856 = DIRECTION ( 'NONE',  ( 0.000000000000000000, 0.000000000000000000, 1.000000000000000000 ) ) ;
#11857 = CARTESIAN_POINT ( 'NONE',  ( 4.189607678530287593, 32.40336399182262284, 53.72836399182268252 ) ) ;
#11858 = AXIS2_PLACEMENT_3D ( 'NONE', #2774, #4357, #16309 ) ;
#11859 = DIRECTION ( 'NONE',  ( 0.000000000000000000, 0.000000000000000000, -1.000000000000000000 ) ) ;
#11860 = B_SPLINE_CURVE_WITH_KNOTS ( 'NONE', 3,
 ( #11678, #5813, #3063, #16598 ),
 .UNSPECIFIED., .F., .F.,
 ( 4, 4 ),
 ( 0.000000000000000000, 1.000000000000000000 ),
 .UNSPECIFIED. ) ;
#11861 = APPLICATION_PROTOCOL_DEFINITION ( 'draft international standard', 'automotive_design', 1998, #13704 ) ;
#11862 = DIRECTION ( 'NONE',  ( 1.000000000000000000, -0.000000000000000000, -0.000000000000000000 ) ) ;
#11863 = EDGE_CURVE ( 'NONE', #14224, #12569, #18287, .T. ) ;
#11864 = EDGE_CURVE ( 'NONE', #72, #17032, #16604, .T. ) ;
#11865 = CARTESIAN_POINT ( 'NONE',  ( -12.35725562635143682, -19.75228648362908501, 36.20117750791695954 ) ) ;
#11866 = PLANE ( 'NONE',  #6452 ) ;
#11868 = EDGE_CURVE ( 'NONE', #5783, #2933, #17498, .T. ) ;
#11867 = CARTESIAN_POINT ( 'NONE',  ( -16.50457296725820555, -28.95583473709189448, 7.107427507916955989 ) ) ;
#11869 = VECTOR ( 'NONE', #14704, 1000.000000000000000 ) ;
#11870 = DIRECTION ( 'NONE',  ( 1.000000000000000000, 0.000000000000000000, 0.000000000000000000 ) ) ;
#11871 = EDGE_LOOP ( 'NONE', ( #11746, #6835, #17974, #3836 ) ) ;
#11872 = CARTESIAN_POINT ( 'NONE',  ( -13.82508104294702100, -18.95583473709188382, 6.455072492083041347 ) ) ;
#11873 = AXIS2_PLACEMENT_3D ( 'NONE', #17456, #5415, #3935 ) ;
#11874 = CARTESIAN_POINT ( 'NONE',  ( -8.044165262908075320, -26.04047135212042718, 5.794927507916956877 ) ) ;
#11875 = VECTOR ( 'NONE', #2731, 1000.000000000000000 ) ;
#11876 = CARTESIAN_POINT ( 'NONE',  ( -1.461580736456473906, 65.46158073645646880, 45.45000000109246940 ) ) ;
#11877 = CARTESIAN_POINT ( 'NONE',  ( -12.04416526290808420, -23.03132541760398766, 7.330072492083044011 ) ) ;
#11878 = CARTESIAN_POINT ( 'NONE',  ( -32.50000000000000000, 53.00000000000000711, -35.00000000000000000 ) ) ;
#11879 = ORIENTED_EDGE ( 'NONE', *, *, #11265, .T. ) ;
#11880 = EDGE_CURVE ( 'NONE', #10268, #8981, #14937, .T. ) ;
#11881 = VECTOR ( 'NONE', #4821, 1000.000000000000000 ) ;
#11882 = CARTESIAN_POINT ( 'NONE',  ( -10.14139447615844425, -21.69985965322670296, -1.842058582391767589E-17 ) ) ;
#11883 = EDGE_LOOP ( 'NONE', ( #13907, #11981 ) ) ;
#11884 = CARTESIAN_POINT ( 'NONE',  ( 4.189131392896579875, 32.57932772728315740, 53.90500129688597042 ) ) ;
#11885 = EDGE_CURVE ( 'NONE', #12460, #13544, #13449, .T. ) ;
#11886 = CARTESIAN_POINT ( 'NONE',  ( -13.25000000000000178, -35.50000000000000000, 5.500000000000000000 ) ) ;
#11887 = CARTESIAN_POINT ( 'NONE',  ( 2.500000000000001776, 64.00000000000000000, 45.59999999999999432 ) ) ;
#11888 = DIRECTION ( 'NONE',  ( 0.000000000000000000, 0.000000000000000000, -1.000000000000000000 ) ) ;
#11889 = CARTESIAN_POINT ( 'NONE',  ( 3.000000000000000888, 2.750000000000000000, 0.000000000000000000 ) ) ;
#11890 = VECTOR ( 'NONE', #7933, 1000.000000000000000 ) ;
#11891 = CARTESIAN_POINT ( 'NONE',  ( -1.461580736456473462, 62.53841926354353120, 47.45000000109246230 ) ) ;
#11892 = VECTOR ( 'NONE', #8417, 1000.000000000000000 ) ;
#11893 = DIRECTION ( 'NONE',  ( 0.000000000000000000, 0.000000000000000000, 1.000000000000000000 ) ) ;
#11894 = EDGE_CURVE ( 'NONE', #11839, #12989, #16202, .T. ) ;
#11895 = CARTESIAN_POINT ( 'NONE',  ( 1.035533905932738197, 66.50000000000000000, 45.75000000000000000 ) ) ;
#11896 = CARTESIAN_POINT ( 'NONE',  ( 4.189131392896553230, 26.90500129688588871, 59.57932772728319293 ) ) ;
#11897 = VECTOR ( 'NONE', #10997, 1000.000000000000114 ) ;
#11898 = ORIENTED_EDGE ( 'NONE', *, *, #16344, .F. ) ;
#11899 = VECTOR ( 'NONE', #16779, 1000.000000000000000 ) ;
#11900 = DIRECTION ( 'NONE',  ( 0.000000000000000000, -1.000000000000000000, 0.000000000000000000 ) ) ;
#11901 = CARTESIAN_POINT ( 'NONE',  ( -17.35725562635144215, -19.58745947852648683, 14.32617750791695777 ) ) ;
#11902 = CARTESIAN_POINT ( 'NONE',  ( -41.00000000000000711, 53.00000000000000711, -25.50000000000000000 ) ) ;
#11903 = CARTESIAN_POINT ( 'NONE',  ( -10.04416526290808953, -22.49542703274172695, 2.080072492083040903 ) ) ;
#11904 = VECTOR ( 'NONE', #11836, 1000.000000000000000 ) ;
#11905 = EDGE_CURVE ( 'NONE', #6698, #6791, #1406, .T. ) ;
#11906 = EDGE_CURVE ( 'NONE', #7234, #17473, #4549, .T. ) ;
#11907 = LINE ( 'NONE', #5248, #15729 ) ;
#11908 = CARTESIAN_POINT ( 'NONE',  ( -17.35725562635144215, -19.58745947852648683, 9.076177507916957765 ) ) ;
#11909 = DIRECTION ( 'NONE',  ( 1.000000000000000000, 0.000000000000000000, -0.000000000000000000 ) ) ;
#11910 = CARTESIAN_POINT ( 'NONE',  ( -10.04416526290807710, -25.50457296725819489, 11.04492750791695599 ) ) ;
#11911 = DIRECTION ( 'NONE',  ( -0.000000000000000000, -1.000000000000000000, -0.000000000000000000 ) ) ;
#11912 = VECTOR ( 'NONE', #11439, 1000.000000000000000 ) ;
#11913 = ADVANCED_FACE ( 'NONE', ( #1609 ), #3170, .T. ) ;
#11914 = CARTESIAN_POINT ( 'NONE',  ( -24.00000000000000711, 110.0000000000000000, -24.49999999999999645 ) ) ;
#11915 = DIRECTION ( 'NONE',  ( -1.000000000000000000, 0.000000000000000000, 0.000000000000000000 ) ) ;
#11916 = PLANE ( 'NONE',  #10044 ) ;
#11917 = VECTOR ( 'NONE', #19035, 1000.000000000000000 ) ;
#11918 = CARTESIAN_POINT ( 'NONE',  ( -0.8561741729129461742, 66.06698730000000808, 46.40000000109247225 ) ) ;
#11919 = DIRECTION ( 'NONE',  ( 0.000000000000000000, -0.000000000000000000, -1.000000000000000000 ) ) ;
#11920 = AXIS2_PLACEMENT_3D ( 'NONE', #8905, #1757, #16257 ) ;
#11921 = DIRECTION ( 'NONE',  ( 0.000000000000000000, 0.7071067811865497932, -0.7071067811865452413 ) ) ;
#11922 = ORIENTED_EDGE ( 'NONE', *, *, #5765, .T. ) ;
#11923 = EDGE_LOOP ( 'NONE', ( #3554, #9194, #10902, #9530 ) ) ;
#11924 = CARTESIAN_POINT ( 'NONE',  ( -21.95583473709189803, -26.04047135212049469, 15.20507249208304046 ) ) ;
#11925 = CARTESIAN_POINT ( 'NONE',  ( 0.000000000000000000, 0.000000000000000000, 30.00000000000000000 ) ) ;
#11927 = ORIENTED_EDGE ( 'NONE', *, *, #13679, .T. ) ;
#11926 = EDGE_LOOP ( 'NONE', ( #1314, #4340, #11959, #12531 ) ) ;
#11928 = PRODUCT_DEFINITION_SHAPE ( 'NONE', 'NONE',  #19401 ) ;
#11929 = EDGE_CURVE ( 'NONE', #12743, #5230, #18077, .T. ) ;
#11930 = CARTESIAN_POINT ( 'NONE',  ( -12.92450931948788906, -26.31681416490114245, 21.98242750791695954 ) ) ;
#11931 = CARTESIAN_POINT ( 'NONE',  ( -44.99999999999998579, 6.000000000000000000, -55.00000000000000000 ) ) ;
#11932 = CARTESIAN_POINT ( 'NONE',  ( -17.04047135212050890, -17.04416526290807710, 11.26757249208304046 ) ) ;
#11933 = CIRCLE ( 'NONE', #13835, 1.500000000000001332 ) ;
#11934 = CARTESIAN_POINT ( 'NONE',  ( -25.00000000000000000, 53.00000000000000711, 30.00000000000000000 ) ) ;
#11935 = CARTESIAN_POINT ( 'NONE',  ( 1.767766952966369987, 65.76776695296638309, 45.00000000218494733 ) ) ;
#11936 = ORIENTED_EDGE ( 'NONE', *, *, #12920, .F. ) ;
#11937 = EDGE_LOOP ( 'NONE', ( #13204, #9784, #17617, #18901, #4695, #14908, #2429, #9619 ) ) ;
#11938 = VECTOR ( 'NONE', #6390, 1000.000000000000114 ) ;
#11939 = CARTESIAN_POINT ( 'NONE',  ( -25.00000000000001421, 107.3545527679194436, 47.49999999999997868 ) ) ;
#11940 = DIRECTION ( 'NONE',  ( -0.000000000000000000, 1.000000000000000000, -0.000000000000000000 ) ) ;
#11941 = ORIENTED_EDGE ( 'NONE', *, *, #7715, .T. ) ;
#11942 = LINE ( 'NONE', #3021, #14361 ) ;
#11943 = CARTESIAN_POINT ( 'NONE',  ( 2.500000000000000000, 1.178949249685212974, -2.042000000000001148 ) ) ;
#11944 = CARTESIAN_POINT ( 'NONE',  ( 2.066987300000001859, 64.85617417291294373, 47.00000000109246656 ) ) ;
#11945 = DIRECTION ( 'NONE',  ( 0.000000000000000000, -0.7071067811865493491, 0.7071067811865457964 ) ) ;
#11946 = VECTOR ( 'NONE', #8103, 1000.000000000000114 ) ;
#11947 = CARTESIAN_POINT ( 'NONE',  ( -41.00000000000000711, 53.00000000000000711, -19.00000000000000000 ) ) ;
#11948 = ORIENTED_EDGE ( 'NONE', *, *, #14966, .F. ) ;
#11950 = ORIENTED_EDGE ( 'NONE', *, *, #1001, .T. ) ;
#11949 = VERTEX_POINT ( 'NONE', #15132 ) ;
#11951 = CARTESIAN_POINT ( 'NONE',  ( -15.16482700510258574, -30.99999999999998224, 22.63867750791695954 ) ) ;
#11952 = VECTOR ( 'NONE', #18204, 1000.000000000000000 ) ;
#11953 = CARTESIAN_POINT ( 'NONE',  ( -2.500000000000001776, 64.00000000000000000, 45.19999999999999574 ) ) ;
#11954 = ORIENTED_EDGE ( 'NONE', *, *, #3264, .F. ) ;
#11955 = ORIENTED_EDGE ( 'NONE', *, *, #8652, .F. ) ;
#11956 = CARTESIAN_POINT ( 'NONE',  ( -14.03132541760400009, -26.95583473709189448, 24.39257249208304046 ) ) ;
#11957 = LINE ( 'NONE', #16176, #13437 ) ;
#11958 = DIRECTION ( 'NONE',  ( 0.000000000000000000, 0.000000000000000000, 1.000000000000000000 ) ) ;
#11959 = ORIENTED_EDGE ( 'NONE', *, *, #12811, .F. ) ;
#11960 = CARTESIAN_POINT ( 'NONE',  ( -15.96867458239599635, -21.04416526290806999, 42.76757249208304756 ) ) ;
#11961 = ORIENTED_EDGE ( 'NONE', *, *, #5180, .T. ) ;
#11962 = DIRECTION ( 'NONE',  ( 0.000000000000000000, -0.5000000000000009992, -0.8660254037844380415 ) ) ;
#11963 = EDGE_LOOP ( 'NONE', ( #7533, #4501, #5736, #15766 ) ) ;
#11964 = DIRECTION ( 'NONE',  ( -0.000000000000000000, -1.000000000000000000, -0.000000000000000000 ) ) ;
#11965 = PLANE ( 'NONE',  #7048 ) ;
#11966 = LINE ( 'NONE', #7459, #6923 ) ;
#11967 = DIRECTION ( 'NONE',  ( 0.000000000000000000, 0.000000000000000000, 1.000000000000000000 ) ) ;
#11968 = CARTESIAN_POINT ( 'NONE',  ( -4.072081901468836307, 26.82127119883319466, 59.66337542264477634 ) ) ;
#11969 = CIRCLE ( 'NONE', #18248, 2.999999999999999112 ) ;
#11970 = DIRECTION ( 'NONE',  ( 0.000000000000000000, 0.000000000000000000, 1.000000000000000000 ) ) ;
#11971 = CARTESIAN_POINT ( 'NONE',  ( -10.75228648362910100, -26.64274437364854009, 21.76367750791695599 ) ) ;
#11972 = CARTESIAN_POINT ( 'NONE',  ( 0.000000000000000000, 64.00000000000000000, 49.99999999999999289 ) ) ;
#11973 = ORIENTED_EDGE ( 'NONE', *, *, #11863, .F. ) ;
#11974 = CARTESIAN_POINT ( 'NONE',  ( -12.64274437364858628, -19.58745947852646552, 22.42382249208304401 ) ) ;
#11975 = FACE_OUTER_BOUND ( 'NONE', #9519, .T. ) ;
#11976 = EDGE_CURVE ( 'NONE', #12423, #1050, #18377, .T. ) ;
#11977 = CARTESIAN_POINT ( 'NONE',  ( -17.99999999999999645, -24.16482700510260173, 10.17382249208304223 ) ) ;
#11978 = CARTESIAN_POINT ( 'NONE',  ( -3.065533689247737392, -43.60761626555502346, 1.500000000000000000 ) ) ;
#11979 = ORIENTED_EDGE ( 'NONE', *, *, #19083, .T. ) ;
#11980 = CARTESIAN_POINT ( 'NONE',  ( -10.31147837279037738, -22.25502639194775512, -4.119453415160654225E-17 ) ) ;
#11981 = ORIENTED_EDGE ( 'NONE', *, *, #16011, .T. ) ;
#11982 = CARTESIAN_POINT ( 'NONE',  ( -17.35725562635144215, -19.58745947852648683, 40.57617750791696665 ) ) ;
#11983 = EDGE_CURVE ( 'NONE', #8044, #7340, #14041, .T. ) ;
#11984 = DIRECTION ( 'NONE',  ( 0.000000000000000000, 1.000000000000000000, -0.000000000000000000 ) ) ;
#11985 = LINE ( 'NONE', #17977, #12792 ) ;
#11986 = CARTESIAN_POINT ( 'NONE',  ( -45.00000000000000000, -1.285879139104706187E-16, 54.99999999999998579 ) ) ;
#11987 = CARTESIAN_POINT ( 'NONE',  ( 1.461580736456473684, 65.46158073645646880, 46.25000000109246656 ) ) ;
#11988 = EDGE_CURVE ( 'NONE', #3590, #17715, #18571, .T. ) ;
#11989 = PLANE ( 'NONE',  #15165 ) ;
#11990 = CARTESIAN_POINT ( 'NONE',  ( -1.035533905932738641, 66.50000000000000000, 48.24999999999999289 ) ) ;
#11991 = DIRECTION ( 'NONE',  ( 0.000000000000000000, -1.000000000000000000, 0.000000000000000000 ) ) ;
#11992 = ORIENTED_EDGE ( 'NONE', *, *, #6786, .F. ) ;
#11993 = DIRECTION ( 'NONE',  ( 6.123233995736766036E-17, 1.000000000000000000, 0.000000000000000000 ) ) ;
#11994 = CARTESIAN_POINT ( 'NONE',  ( -14.83517299489739649, -18.99999999999997868, 14.76367750791695777 ) ) ;
#11995 = CARTESIAN_POINT ( 'NONE',  ( -1.035533905932738863, 61.50000000000000000, 48.65000000218493881 ) ) ;
#11996 = ADVANCED_FACE ( 'NONE', ( #6315 ), #15027, .F. ) ;
#11997 = CARTESIAN_POINT ( 'NONE',  ( -20.04416526290809131, -22.82508104294699791, 10.39257249208304223 ) ) ;
#11998 = LINE ( 'NONE', #11803, #17291 ) ;
#11999 = CARTESIAN_POINT ( 'NONE',  ( -16.50457296725820555, -28.95583473709189448, 7.107427507916955989 ) ) ;
#12000 = CARTESIAN_POINT ( 'NONE',  ( -40.00000000000000711, 110.0000000000000000, -45.00000000000000000 ) ) ;
#12001 = CARTESIAN_POINT ( 'NONE',  ( -17.64274437364855430, -28.24771351637087236, 17.82617750791695599 ) ) ;
#12002 = CARTESIAN_POINT ( 'NONE',  ( -9.575581032440643243E-15, 24.93431457505072402, 61.55096679918780467 ) ) ;
#12003 = LINE ( 'NONE', #10337, #17495 ) ;
#12004 = LINE ( 'NONE', #7709, #4660 ) ;
#12005 = SHAPE_REPRESENTATION ( 'Spring-Loaded Carriage Elevator Arm', ( #1791 ), #13038 ) ;
#12006 = CARTESIAN_POINT ( 'NONE',  ( -25.00000000000001421, 0.000000000000000000, 47.49999999999997868 ) ) ;
#12007 = CARTESIAN_POINT ( 'NONE',  ( -1.265664690411616068E-16, 66.06698730000000808, 45.55000000109246372 ) ) ;
#12008 = CARTESIAN_POINT ( 'NONE',  ( 7.500000000000005329, -26.00000000000000000, 4.500000000000000888 ) ) ;
#12009 = EDGE_CURVE ( 'NONE', #1553, #6936, #4944, .T. ) ;
#12010 = EDGE_CURVE ( 'NONE', #76, #3347, #3464, .T. ) ;
#12011 = CIRCLE ( 'NONE', #14521, 1.249999999999999334 ) ;
#12012 = CARTESIAN_POINT ( 'NONE',  ( -19.99999999999999645, -52.00000000000000711, 0.000000000000000000 ) ) ;
#12013 = ORIENTED_EDGE ( 'NONE', *, *, #14159, .F. ) ;
#12014 = ORIENTED_EDGE ( 'NONE', *, *, #16599, .T. ) ;
#12015 = EDGE_CURVE ( 'NONE', #18408, #10469, #3270, .T. ) ;
#12016 = CARTESIAN_POINT ( 'NONE',  ( -14.83517299489734853, -30.99999999999998224, 24.61132249208304046 ) ) ;
#12017 = SURFACE_SIDE_STYLE ('',( #16438 ) ) ;
#12018 = ADVANCED_BREP_SHAPE_REPRESENTATION ( '', ( #3958, #1791 ), #12745 ) ;
#12019 = CARTESIAN_POINT ( 'NONE',  ( -13.82508104294702100, -18.95583473709188382, 1.205072492083040903 ) ) ;
#12021 = ORIENTED_EDGE ( 'NONE', *, *, #18128, .F. ) ;
#12020 = ORIENTED_EDGE ( 'NONE', *, *, #9631, .F. ) ;
#12022 = CARTESIAN_POINT ( 'NONE',  ( -17.31681416490115311, -26.07549068051209318, 12.79492750791696132 ) ) ;
#12023 = DIRECTION ( 'NONE',  ( 0.000000000000000000, 0.000000000000000000, 1.000000000000000000 ) ) ;
#12024 = CARTESIAN_POINT ( 'NONE',  ( -14.83517299489740715, -16.99999999999997868, 41.01367750791695954 ) ) ;
#12025 = CARTESIAN_POINT ( 'NONE',  ( 1.767766952966369987, 65.76776695296638309, 48.09999999999999432 ) ) ;
#12026 = CARTESIAN_POINT ( 'NONE',  ( 1.461580736456473684, 65.46158073645646880, 47.65000000109247225 ) ) ;
#12027 = ORIENTED_EDGE ( 'NONE', *, *, #19318, .T. ) ;
#12028 = VERTEX_POINT ( 'NONE', #2092 ) ;
#12029 = COLOUR_RGB ( '', 0.72549020, 0.75294118, 0.79215686) ;
#12030 = CARTESIAN_POINT ( 'NONE',  ( 24.99999999999998579, -6.000000000000000000, 47.49999999999997868 ) ) ;
#12031 = CARTESIAN_POINT ( 'NONE',  ( 41.99999999999997868, 139.6861997365471950, 51.99999999999997868 ) ) ;
#12032 = VECTOR ( 'NONE', #16404, 1000.000000000000000 ) ;
#12033 = ORIENTED_EDGE ( 'NONE', *, *, #3458, .F. ) ;
#12034 = DIRECTION ( 'NONE',  ( 1.000000000000000000, 0.000000000000000000, 0.000000000000000000 ) ) ;
#12035 = CARTESIAN_POINT ( 'NONE',  ( -10.00000000000000000, -0.000000000000000000, 37.00000000000000000 ) ) ;
#12036 = CARTESIAN_POINT ( 'NONE',  ( 0.8561741729129460632, 66.06698729999999387, 48.70000000109247651 ) ) ;
#12037 = EDGE_CURVE ( 'NONE', #18125, #8404, #4756, .T. ) ;
#12038 = EDGE_CURVE ( 'NONE', #6946, #16414, #16258, .T. ) ;
#12039 = CARTESIAN_POINT ( 'NONE',  ( 0.1499999999999973577, 0.000000000000000000, 0.000000000000000000 ) ) ;
#12040 = DIRECTION ( 'NONE',  ( -0.000000000000000000, -1.000000000000000000, -0.000000000000000000 ) ) ;
#12041 = VERTEX_POINT ( 'NONE', #2181 ) ;
#12043 = ORIENTED_EDGE ( 'NONE', *, *, #11767, .F. ) ;
#12042 = ORIENTED_EDGE ( 'NONE', *, *, #10732, .F. ) ;
#12044 = CARTESIAN_POINT ( 'NONE',  ( -21.14459132904236327, -27.35725562635143149, 13.01367750791695777 ) ) ;
#12045 = VERTEX_POINT ( 'NONE', #3616 ) ;
#12046 = CARTESIAN_POINT ( 'NONE',  ( -44.99999999999998579, 3.000000000000000000, -53.40000000000000568 ) ) ;
#12047 = ORIENTED_EDGE ( 'NONE', *, *, #1569, .F. ) ;
#12048 = VECTOR ( 'NONE', #3659, 1000.000000000000000 ) ;
#12049 = EDGE_LOOP ( 'NONE', ( #2454, #13796, #3269, #4089 ) ) ;
#12050 = CARTESIAN_POINT ( 'NONE',  ( -17.95583473709190869, -24.96867458239598037, 15.20507249208304579 ) ) ;
#12051 = PLANE ( 'NONE',  #8144 ) ;
#12052 = DIRECTION ( 'NONE',  ( -0.000000000000000000, -0.000000000000000000, -1.000000000000000000 ) ) ;
#12053 = ORIENTED_EDGE ( 'NONE', *, *, #17919, .F. ) ;
#12054 = CARTESIAN_POINT ( 'NONE',  ( -17.99999999999999645, -23.83517299489736985, 18.70117750791695599 ) ) ;
#12055 = CARTESIAN_POINT ( 'NONE',  ( 2.500000000000001776, 64.00000000000000000, 47.30000000218494449 ) ) ;
#12056 = VERTEX_POINT ( 'NONE', #716 ) ;
#12057 = CARTESIAN_POINT ( 'NONE',  ( -1.040834085586084257E-14, 27.62132034355962773, 54.62132034355965260 ) ) ;
#12058 = ORIENTED_EDGE ( 'NONE', *, *, #18875, .F. ) ;
#12059 = LINE ( 'NONE', #7660, #16619 ) ;
#12060 = LINE ( 'NONE', #16184, #14880 ) ;
#12061 = AXIS2_PLACEMENT_3D ( 'NONE', #16991, #601, #15220 ) ;
#12062 = DIRECTION ( 'NONE',  ( 0.000000000000000000, 0.000000000000000000, -1.000000000000000000 ) ) ;
#12063 = VECTOR ( 'NONE', #18514, 1000.000000000000000 ) ;
#12064 = EDGE_CURVE ( 'NONE', #1874, #15591, #8171, .T. ) ;
#12065 = CARTESIAN_POINT ( 'NONE',  ( -6.528048594804060301, -45.28611686177728046, 3.000000000000000000 ) ) ;
#12066 = CARTESIAN_POINT ( 'NONE',  ( -41.00000000000000711, 113.0000000000000000, -50.00000000000000000 ) ) ;
#12067 = DIRECTION ( 'NONE',  ( -0.9863224920830415687, -6.560347287104328168E-15, -0.1648270051026180794 ) ) ;
#12068 = CARTESIAN_POINT ( 'NONE',  ( -9.955834737091912245, -22.82508104294696594, 15.85742750791695777 ) ) ;
#12069 = CARTESIAN_POINT ( 'NONE',  ( -0.9999999999999945599, -32.00000000000000000, 9.500000000000001776 ) ) ;
#12070 = ORIENTED_EDGE ( 'NONE', *, *, #15140, .T. ) ;
#12071 = CARTESIAN_POINT ( 'NONE',  ( -16.17491895705296656, -29.04416526290807710, 24.83007249208304046 ) ) ;
#12072 =( REPRESENTATION_RELATIONSHIP ('NONE','NONE', #7912, #15908 ) REPRESENTATION_RELATIONSHIP_WITH_TRANSFORMATION ( #15482 )SHAPE_REPRESENTATION_RELATIONSHIP( ) );
#12073 = AXIS2_PLACEMENT_3D ( 'NONE', #5144, #14965, #18482 ) ;
#12074 = VECTOR ( 'NONE', #14947, 1000.000000000000000 ) ;
#12075 = CARTESIAN_POINT ( 'NONE',  ( -1.265664690411616068E-16, 66.06698730000000808, 44.55000000109247082 ) ) ;
#12076 = CARTESIAN_POINT ( 'NONE',  ( -13.35725562635141195, -26.51566270880198672, 24.17382249208304046 ) ) ;
#12077 = DIRECTION ( 'NONE',  ( -1.000000000000000000, 0.000000000000000000, 0.000000000000000000 ) ) ;
#12078 = ORIENTED_EDGE ( 'NONE', *, *, #18199, .T. ) ;
#12079 = DIRECTION ( 'NONE',  ( -0.000000000000000000, -0.000000000000000000, -1.000000000000000000 ) ) ;
#12080 = EDGE_LOOP ( 'NONE', ( #18715, #18108, #14313, #13800 ) ) ;
#12081 = FACE_OUTER_BOUND ( 'NONE', #11759, .T. ) ;
#12082 = CARTESIAN_POINT ( 'NONE',  ( -14.99999999999999645, 73.00000000000001421, 20.99999999999998224 ) ) ;
#12083 = CARTESIAN_POINT ( 'NONE',  ( 1.300000000000000044, 0.000000000000000000, 1.280000000000000027 ) ) ;
#12084 = EDGE_CURVE ( 'NONE', #18422, #9008, #6608, .T. ) ;
#12085 = CARTESIAN_POINT ( 'NONE',  ( 1.461580736456473906, 62.53841926354353120, 48.45000000109246940 ) ) ;
#12086 = VECTOR ( 'NONE', #9912, 1000.000000000000114 ) ;
#12087 = AXIS2_PLACEMENT_3D ( 'NONE', #4767, #16713, #3281 ) ;
#12088 = CARTESIAN_POINT ( 'NONE',  ( -1.530808498934192803E-16, 66.50000000000000000, 46.59999999999999432 ) ) ;
#12089 = LINE ( 'NONE', #1808, #4263 ) ;
#12090 = ORIENTED_EDGE ( 'NONE', *, *, #18143, .T. ) ;
#12091 = DIRECTION ( 'NONE',  ( 6.123233995736766036E-17, 1.000000000000000000, 0.000000000000000000 ) ) ;
#12092 = CARTESIAN_POINT ( 'NONE',  ( -19.41254052147348830, -26.35725562635142083, 23.51367750791695954 ) ) ;
#12093 = CARTESIAN_POINT ( 'NONE',  ( -16.17491895705301275, -18.95583473709189803, 9.294927507916954212 ) ) ;
#12094 = CARTESIAN_POINT ( 'NONE',  ( -1.366617256750952913, 65.93762474262220508, 45.00000000000000711 ) ) ;
#12095 = CARTESIAN_POINT ( 'NONE',  ( -10.58745947852648328, -26.35725562635138530, 7.986322492083041347 ) ) ;
#12096 = STYLED_ITEM ( 'NONE', ( #12438 ), #571 ) ;
#12097 = VECTOR ( 'NONE', #1537, 1000.000000000000000 ) ;
#12098 = CARTESIAN_POINT ( 'NONE',  ( -0.8561741729129461742, 66.06698729999999387, 45.60000000109246088 ) ) ;
#12099 = CARTESIAN_POINT ( 'NONE',  ( -10.04416526290807710, -25.50457296725819489, 0.5449275079169579872 ) ) ;
#12100 = CARTESIAN_POINT ( 'NONE',  ( 50.00000000000000000, 118.0000000000000142, -56.99999999999999289 ) ) ;
#12101 = CARTESIAN_POINT ( 'NONE',  ( -17.35725562635144215, -19.58745947852648683, 24.82617750791695954 ) ) ;
#12102 = LINE ( 'NONE', #19274, #18455 ) ;
#12103 = CARTESIAN_POINT ( 'NONE',  ( 0.000000000000000000, 64.00000000000000000, 49.99999999999999289 ) ) ;
#12104 = CARTESIAN_POINT ( 'NONE',  ( -2.066987300000001859, 64.85617417291294373, 46.50000000109246656 ) ) ;
#12105 = FACE_OUTER_BOUND ( 'NONE', #7682, .T. ) ;
#12106 = DIRECTION ( 'NONE',  ( 0.000000000000000000, 0.000000000000000000, -1.000000000000000000 ) ) ;
#12107 = LINE ( 'NONE', #7311, #1778 ) ;
#12108 = CARTESIAN_POINT ( 'NONE',  ( 0.8561741729129460632, 66.06698729999999387, 49.50000000109246656 ) ) ;
#12109 = EDGE_CURVE ( 'NONE', #14374, #11453, #13852, .T. ) ;
#12110 = EDGE_CURVE ( 'NONE', #17649, #3686, #12467, .T. ) ;
#12111 = DIRECTION ( 'NONE',  ( 0.000000000000000000, 0.000000000000000000, 1.000000000000000000 ) ) ;
#12112 =( GEOMETRIC_REPRESENTATION_CONTEXT ( 3 ) GLOBAL_UNCERTAINTY_ASSIGNED_CONTEXT ( ( #439 ) ) GLOBAL_UNIT_ASSIGNED_CONTEXT ( ( #14477, #7025, #5561 ) ) REPRESENTATION_CONTEXT ( 'NONE', 'WORKASPACE' ) );
#12113 = DIRECTION ( 'NONE',  ( -2.220446049250312588E-16, 0.7071067811865453523, 0.7071067811865496822 ) ) ;
#12114 = VERTEX_POINT ( 'NONE', #17000 ) ;
#12115 = ORIENTED_EDGE ( 'NONE', *, *, #17994, .T. ) ;
#12116 = CARTESIAN_POINT ( 'NONE',  ( -11.64274437364859693, -17.85540867095757989, 11.92382249208304046 ) ) ;
#12117 =( NAMED_UNIT ( * ) SI_UNIT ( $, .STERADIAN. ) SOLID_ANGLE_UNIT ( ) );
#12118 = CARTESIAN_POINT ( 'NONE',  ( -19.95583473709190514, -25.50457296725823042, 15.20507249208304046 ) ) ;
#12120 = EDGE_LOOP ( 'NONE', ( #10569, #6153, #7543, #8513 ) ) ;
#12119 = EDGE_LOOP ( 'NONE', ( #4431, #5807, #18626, #12149, #6444 ) ) ;
#12121 = CARTESIAN_POINT ( 'NONE',  ( -11.99999999999999289, -24.16482700510258752, 16.07617750791696309 ) ) ;
#12122 = FACE_OUTER_BOUND ( 'NONE', #16342, .T. ) ;
#12123 = CARTESIAN_POINT ( 'NONE',  ( -9.754982604823302594, -29.00369391078756465, 8.205072492083040459 ) ) ;
#12124 = CARTESIAN_POINT ( 'NONE',  ( -1.040834085586084257E-14, 27.62132034355962773, 54.62132034355965260 ) ) ;
#12125 = CARTESIAN_POINT ( 'NONE',  ( 2.066987300000001859, 64.85617417291294373, 46.00000000109246656 ) ) ;
#12126 = EDGE_LOOP ( 'NONE', ( #17182, #15580, #18215, #17360 ) ) ;
#12127 = ORIENTED_EDGE ( 'NONE', *, *, #11265, .F. ) ;
#12128 =( BOUNDED_CURVE ( )  B_SPLINE_CURVE ( 2, ( #213, #3248, #16685, #1976, #15113, #6293, #12156, #4828, #10586 ),
 .UNSPECIFIED., .F., .F. ) 
 B_SPLINE_CURVE_WITH_KNOTS ( ( 3, 2, 2, 2, 3 ),
 ( 0.5714285714285713969, 0.5892857142857143016, 0.6071428571428569843, 0.6249999999999998890, 0.6428571428571427937 ),
 .UNSPECIFIED. ) 
 CURVE ( )  GEOMETRIC_REPRESENTATION_ITEM ( )  RATIONAL_B_SPLINE_CURVE ( ( 1.000000000000000000, 0.9238795325112867385, 1.000000000000000000, 0.9238795325112867385, 1.000000000000000000, 0.9238795325112867385, 1.000000000000000000, 0.9238795325112871826, 0.9999999999999995559 ) ) 
 REPRESENTATION_ITEM ( '' )  );
#12129 = CARTESIAN_POINT ( 'NONE',  ( -1.035533905932738641, 66.50000000000000000, 45.95000000218494307 ) ) ;
#12130 = ORIENTED_EDGE ( 'NONE', *, *, #217, .T. ) ;
#12131 = EDGE_CURVE ( 'NONE', #10270, #11147, #13759, .T. ) ;
#12132 = ORIENTED_EDGE ( 'NONE', *, *, #11034, .F. ) ;
#12133 = CARTESIAN_POINT ( 'NONE',  ( 3.099999999999998757, 0.000000000000000000, 0.000000000000000000 ) ) ;
#12134 = CARTESIAN_POINT ( 'NONE',  ( 7.500000000000005329, -38.00000000000000000, 1.500000000000000000 ) ) ;
#12135 = EDGE_CURVE ( 'NONE', #15077, #5315, #9625, .T. ) ;
#12136 = CARTESIAN_POINT ( 'NONE',  ( 2.066987300000002303, 63.14382582708705627, 46.10000000109246798 ) ) ;
#12137 = LINE ( 'NONE', #3027, #5644 ) ;
#12138 = LINE ( 'NONE', #9298, #6139 ) ;
#12139 = VERTEX_POINT ( 'NONE', #10709 ) ;
#12141 = ORIENTED_EDGE ( 'NONE', *, *, #3310, .T. ) ;
#12140 = VERTEX_POINT ( 'NONE', #10803 ) ;
#12142 = CARTESIAN_POINT ( 'NONE',  ( -9.996306089212364299, -29.24501739517662813, 16.73242750791695954 ) ) ;
#12143 = FILL_AREA_STYLE_COLOUR ( '', #11471 ) ;
#12144 = VERTEX_POINT ( 'NONE', #16799 ) ;
#12145 = EDGE_LOOP ( 'NONE', ( #1097, #5673, #1176, #3462 ) ) ;
#12146 = CARTESIAN_POINT ( 'NONE',  ( -11.95583473709190514, -24.63902057219072361, 13.01757249208304401 ) ) ;
#12147 = CARTESIAN_POINT ( 'NONE',  ( 2.066987300000001415, 64.00000000000000000, 49.15000000109247225 ) ) ;
#12148 = LINE ( 'NONE', #19321, #5946 ) ;
#12149 = ORIENTED_EDGE ( 'NONE', *, *, #11472, .F. ) ;
#12150 = CARTESIAN_POINT ( 'NONE',  ( -16.64274437364856496, -26.51566270880199738, 12.57617750791695954 ) ) ;
#12151 = CARTESIAN_POINT ( 'NONE',  ( -50.00000000000001421, 3.000000000000000000, 59.99999999999997868 ) ) ;
#12152 = ORIENTED_EDGE ( 'NONE', *, *, #10101, .T. ) ;
#12153 = ADVANCED_FACE ( 'NONE', ( #9241 ), #15231, .F. ) ;
#12154 = DIRECTION ( 'NONE',  ( -1.000000000000000000, 0.000000000000000000, 0.000000000000000000 ) ) ;
#12155 = VERTEX_POINT ( 'NONE', #7781 ) ;
#12156 = CARTESIAN_POINT ( 'NONE',  ( 1.767766952966369987, 65.76776695296638309, 46.49999999999999289 ) ) ;
#12157 = CARTESIAN_POINT ( 'NONE',  ( -14.99999999999999645, 3.000000000000000000, 26.99999999999997868 ) ) ;
#12158 = FACE_OUTER_BOUND ( 'NONE', #16075, .T. ) ;
#12159 = ADVANCED_FACE ( 'NONE', ( #13748 ), #9332, .T. ) ;
#12160 = DIRECTION ( 'NONE',  ( -8.673617379884027583E-16, 1.000000000000000000, 0.000000000000000000 ) ) ;
#12161 = LINE ( 'NONE', #13336, #14451 ) ;
#12162 = AXIS2_PLACEMENT_3D ( 'NONE', #6905, #2585, #2681 ) ;
#12163 = PRODUCT ( 'BR-818', 'BR-818', '', ( #2655 ) ) ;
#12164 = CARTESIAN_POINT ( 'NONE',  ( -14.83517299489739649, -18.99999999999997868, 41.01367750791696665 ) ) ;
#12165 = PLANE ( 'NONE',  #12061 ) ;
#12166 = ORIENTED_EDGE ( 'NONE', *, *, #1242, .F. ) ;
#12167 = CARTESIAN_POINT ( 'NONE',  ( -19.95583473709191580, -22.49542703274176603, 18.91992750791694888 ) ) ;
#12168 = CARTESIAN_POINT ( 'NONE',  ( 32.50000000000000000, 52.00000000000000711, 15.00000000000000000 ) ) ;
#12169 = ORIENTED_EDGE ( 'NONE', *, *, #19065, .T. ) ;
#12170 = UNCERTAINTY_MEASURE_WITH_UNIT (LENGTH_MEASURE( 1.000000000000000082E-05 ), #14950, 'distance_accuracy_value', 'NONE');
#12171 = CARTESIAN_POINT ( 'NONE',  ( -9.999999999999994671, -23.83517299489734143, 18.04882249208304401 ) ) ;
#12172 = AXIS2_PLACEMENT_3D ( 'NONE', #13510, #6070, #12034 ) ;
#12173 = EDGE_CURVE ( 'NONE', #10794, #3796, #11185, .T. ) ;
#12174 = DIRECTION ( 'NONE',  ( 1.000000000000000000, 0.000000000000000000, 0.000000000000000000 ) ) ;
#12175 = CARTESIAN_POINT ( 'NONE',  ( -14.83517299489736985, -26.99999999999998579, 14.11132249208304223 ) ) ;
#12176 = AXIS2_PLACEMENT_3D ( 'NONE', #13672, #18400, #4780 ) ;
#12177 = CARTESIAN_POINT ( 'NONE',  ( 0.000000000000000000, 64.00000000000000000, 49.99999999999999289 ) ) ;
#12178 = ORIENTED_EDGE ( 'NONE', *, *, #1634, .T. ) ;
#12179 = DIRECTION ( 'NONE',  ( -0.000000000000000000, -0.000000000000000000, -1.000000000000000000 ) ) ;
#12180 = EDGE_LOOP ( 'NONE', ( #10146, #2611, #13915, #9287, #5389, #18657 ) ) ;
#12181 = LINE ( 'NONE', #3172, #7497 ) ;
#12182 = DIRECTION ( 'NONE',  ( -1.000000000000000000, -0.000000000000000000, -0.000000000000000000 ) ) ;
#12183 = CARTESIAN_POINT ( 'NONE',  ( 43.49999999999997868, 115.0000000000000000, -52.50000000000002132 ) ) ;
#12184 = PLANE ( 'NONE',  #273 ) ;
#12185 = VECTOR ( 'NONE', #6317, 1000.000000000000000 ) ;
#12186 = CARTESIAN_POINT ( 'NONE',  ( -1.035533905932738641, 66.50000000000000000, 46.64999999999999858 ) ) ;
#12187 = PRODUCT_RELATED_PRODUCT_CATEGORY ( 'part', '', ( #2850 ) ) ;
#12188 = CARTESIAN_POINT ( 'NONE',  ( 32.50000000000000000, -6.000000000000000000, -25.00000000000001421 ) ) ;
#12189 = AXIS2_PLACEMENT_3D ( 'NONE', #6710, #444, #6429 ) ;
#12190 = VECTOR ( 'NONE', #17045, 1000.000000000000000 ) ;
#12191 = ORIENTED_EDGE ( 'NONE', *, *, #18958, .F. ) ;
#12192 = DIRECTION ( 'NONE',  ( 1.000000000000000000, 0.000000000000000000, 0.000000000000000000 ) ) ;
#12193 = CARTESIAN_POINT ( 'NONE',  ( -16.50457296725820555, -28.95583473709189448, 22.85742750791695954 ) ) ;
#12194 = CARTESIAN_POINT ( 'NONE',  ( 2.500000000000001776, 65.03553390593273775, 47.35000000218494165 ) ) ;
#12195 = CARTESIAN_POINT ( 'NONE',  ( -19.24771351637086880, -26.64274437364857206, 25.48632249208304401 ) ) ;
#12196 = VECTOR ( 'NONE', #3370, 1000.000000000000000 ) ;
#12197 = LINE ( 'NONE', #19365, #11325 ) ;
#12198 = CARTESIAN_POINT ( 'NONE',  ( -19.99999999999999645, -23.83517299489738051, 18.70117750791695954 ) ) ;
#12199 = DIRECTION ( 'NONE',  ( 1.000000000000000000, -0.000000000000000000, -0.000000000000000000 ) ) ;
#12200 = CARTESIAN_POINT ( 'NONE',  ( -19.24771351637089367, -21.35725562635142438, 13.88867750791695954 ) ) ;
#12201 = VECTOR ( 'NONE', #19226, 1000.000000000000000 ) ;
#12202 = CARTESIAN_POINT ( 'NONE',  ( -41.99999999999997868, 3.000000000000000000, 0.000000000000000000 ) ) ;
#12203 = DIRECTION ( 'NONE',  ( 0.000000000000000000, -0.000000000000000000, 1.000000000000000000 ) ) ;
#12204 = CARTESIAN_POINT ( 'NONE',  ( 1.461580736456473906, 62.53841926354353120, 49.25000000109246656 ) ) ;
#12205 = CARTESIAN_POINT ( 'NONE',  ( -41.00000000000000711, 53.00000000000000711, 0.5000000000000004441 ) ) ;
#12206 = CARTESIAN_POINT ( 'NONE',  ( -4.000000000000001776, 67.00000000000000000, 34.99999999999999289 ) ) ;
#12207 = VECTOR ( 'NONE', #688, 1000.000000000000114 ) ;
#12208 = CARTESIAN_POINT ( 'NONE',  ( 2.500000000000001776, 64.00000000000000000, 48.79999999999999716 ) ) ;
#12209 = CARTESIAN_POINT ( 'NONE',  ( -2.066987300000001859, 64.85617417291294373, 46.50000000109246656 ) ) ;
#12210 = DIRECTION ( 'NONE',  ( 0.000000000000000000, 0.5000000000000009992, 0.8660254037844380415 ) ) ;
#12211 = VECTOR ( 'NONE', #14738, 999.9999999999998863 ) ;
#12212 = ORIENTED_EDGE ( 'NONE', *, *, #12280, .T. ) ;
#12213 = ORIENTED_EDGE ( 'NONE', *, *, #4353, .T. ) ;
#12214 = CARTESIAN_POINT ( 'NONE',  ( -21.99999999999999289, -24.16482700510262305, 20.67382249208304046 ) ) ;
#12215 = AXIS2_PLACEMENT_3D ( 'NONE', #412, #5300, #8251 ) ;
#12216 = CARTESIAN_POINT ( 'NONE',  ( -16.17491895705296656, -29.04416526290807354, 9.080072492083038682 ) ) ;
#12217 = EDGE_LOOP ( 'NONE', ( #3620, #16605, #9684, #9978 ) ) ;
#12218 = CARTESIAN_POINT ( 'NONE',  ( -16.35725562635142794, -21.31951028609535470, 9.076177507916959541 ) ) ;
#12219 = CARTESIAN_POINT ( 'NONE',  ( -1.265664690411616068E-16, 66.06698730000000808, 44.55000000109247082 ) ) ;
#12220 = CARTESIAN_POINT ( 'NONE',  ( -16.71081734191520596, -31.04416526290808065, 19.58007249208303691 ) ) ;
#12221 = AXIS2_PLACEMENT_3D ( 'NONE', #11878, #17876, #8848 ) ;
#12222 = CYLINDRICAL_SURFACE ( 'NONE', #4784, 10.00000000000000000 ) ;
#12223 = CARTESIAN_POINT ( 'NONE',  ( -2.066987300000001859, 64.85617417291294373, 45.50000000109247367 ) ) ;
#12224 = ORIENTED_EDGE ( 'NONE', *, *, #10536, .T. ) ;
#12225 = VERTEX_POINT ( 'NONE', #2558 ) ;
#12226 = EDGE_CURVE ( 'NONE', #19128, #1572, #17183, .T. ) ;
#12227 = EDGE_CURVE ( 'NONE', #18340, #10184, #18847, .T. ) ;
#12228 = CARTESIAN_POINT ( 'NONE',  ( -35.00000000000002132, -6.000000000000000000, -42.50000000000001421 ) ) ;
#12229 = EDGE_LOOP ( 'NONE', ( #563, #9819, #10573, #9502 ) ) ;
#12230 = VECTOR ( 'NONE', #12289, 999.9999999999998863 ) ;
#12231 = VERTEX_POINT ( 'NONE', #8354 ) ;
#12232 = CARTESIAN_POINT ( 'NONE',  ( 1.461580736456473906, 62.53841926354353120, 48.25000000109246656 ) ) ;
#12233 = CARTESIAN_POINT ( 'NONE',  ( -24.00000000000000711, 53.00000000000000711, -12.50000000000000000 ) ) ;
#12234 = EDGE_CURVE ( 'NONE', #209, #9274, #7065, .T. ) ;
#12235 = VECTOR ( 'NONE', #3328, 1000.000000000000000 ) ;
#12236 = CARTESIAN_POINT ( 'NONE',  ( 8.000000000000003553, -25.00000000000000711, 1.500000000000000000 ) ) ;
#12237 = LINE ( 'NONE', #13606, #11573 ) ;
#12238 = ADVANCED_FACE ( 'NONE', ( #12663 ), #17557, .T. ) ;
#12239 =( GEOMETRIC_REPRESENTATION_CONTEXT ( 3 ) GLOBAL_UNCERTAINTY_ASSIGNED_CONTEXT ( ( #11384 ) ) GLOBAL_UNIT_ASSIGNED_CONTEXT ( ( #403, #6288, #6481 ) ) REPRESENTATION_CONTEXT ( 'NONE', 'WORKASPACE' ) );
#12240 = PLANE ( 'NONE',  #8613 ) ;
#12241 = EDGE_LOOP ( 'NONE', ( #7619, #13330 ) ) ;
#12243 = ORIENTED_EDGE ( 'NONE', *, *, #13258, .T. ) ;
#12242 = ORIENTED_EDGE ( 'NONE', *, *, #5806, .T. ) ;
#12244 = CARTESIAN_POINT ( 'NONE',  ( -11.35725562635144925, -18.02023567606020293, 20.45117750791695954 ) ) ;
#12245 = VECTOR ( 'NONE', #15215, 1000.000000000000000 ) ;
#12246 = ORIENTED_EDGE ( 'NONE', *, *, #7309, .T. ) ;
#12247 = ORIENTED_EDGE ( 'NONE', *, *, #9388, .F. ) ;
#12248 = CARTESIAN_POINT ( 'NONE',  ( -17.99999999999999645, -24.16482700510260173, 20.67382249208304046 ) ) ;
#12249 = EDGE_CURVE ( 'NONE', #2289, #18664, #6875, .T. ) ;
#12250 = CARTESIAN_POINT ( 'NONE',  ( -13.28918265808472299, -31.04416526290805933, 11.91992750791695777 ) ) ;
#12251 =( BOUNDED_CURVE ( )  B_SPLINE_CURVE ( 2, ( #6873, #1178, #14512, #15892, #1082, #14613, #17554, #19127, #13129 ),
 .UNSPECIFIED., .F., .F. ) 
 B_SPLINE_CURVE_WITH_KNOTS ( ( 3, 2, 2, 2, 3 ),
 ( 0.1428571428571429047, 0.1607142857142857262, 0.1785714285714285476, 0.1964285714285713413, 0.2142857142857141350 ),
 .UNSPECIFIED. ) 
 CURVE ( )  GEOMETRIC_REPRESENTATION_ITEM ( )  RATIONAL_B_SPLINE_CURVE ( ( 0.9999999999999997780, 0.9238795325112869605, 1.000000000000000000, 0.9238795325112867385, 1.000000000000000000, 0.9238795325112867385, 1.000000000000000000, 0.9238795325112872936, 0.9999999999999994449 ) ) 
 REPRESENTATION_ITEM ( '' )  );
#12252 = VECTOR ( 'NONE', #12671, 1000.000000000000000 ) ;
#12253 = CARTESIAN_POINT ( 'NONE',  ( 0.8561741729129460632, 66.06698730000000808, 47.70000000109248361 ) ) ;
#12254 = FACE_OUTER_BOUND ( 'NONE', #9371, .T. ) ;
#12255 = ORIENTED_EDGE ( 'NONE', *, *, #8994, .T. ) ;
#12256 = CARTESIAN_POINT ( 'NONE',  ( -16.64274437364856496, -26.51566270880199738, 17.82617750791695954 ) ) ;
#12257 = VECTOR ( 'NONE', #5455, 1000.000000000000000 ) ;
#12258 = CARTESIAN_POINT ( 'NONE',  ( -24.00000000000000000, 110.0000000000000000, 30.00000000000000000 ) ) ;
#12259 = ORIENTED_EDGE ( 'NONE', *, *, #17800, .F. ) ;
#12260 = CARTESIAN_POINT ( 'NONE',  ( 12.99999999999999822, 0.000000000000000000, 2.055000000000000160 ) ) ;
#12261 = ORIENTED_EDGE ( 'NONE', *, *, #19370, .T. ) ;
#12262 = CARTESIAN_POINT ( 'NONE',  ( -11.75000000000000000, -35.50000000000000000, 5.500000000000000000 ) ) ;
#12263 = FACE_BOUND ( 'NONE', #13086, .T. ) ;
#12264 = DIRECTION ( 'NONE',  ( 0.000000000000000000, 0.5000000000000013323, 0.8660254037844378194 ) ) ;
#12265 = FACE_BOUND ( 'NONE', #230, .T. ) ;
#12266 = CARTESIAN_POINT ( 'NONE',  ( 0.8561741729129460632, 66.06698729999999387, 49.30000000109246372 ) ) ;
#12267 = VECTOR ( 'NONE', #8636, 1000.000000000000000 ) ;
#12268 = CARTESIAN_POINT ( 'NONE',  ( -41.00000000000000711, 110.0000000000000000, -18.00000000000000000 ) ) ;
#12269 = DIRECTION ( 'NONE',  ( 0.000000000000000000, 0.000000000000000000, 1.000000000000000000 ) ) ;
#12270 = AXIS2_PLACEMENT_3D ( 'NONE', #12787, #5360, #11320 ) ;
#12271 = CARTESIAN_POINT ( 'NONE',  ( -10.58745947852649927, -21.64274437364853654, 36.63867750791695954 ) ) ;
#12272 = DIRECTION ( 'NONE',  ( 0.000000000000000000, -1.000000000000000000, -0.000000000000000000 ) ) ;
#12273 = ORIENTED_EDGE ( 'NONE', *, *, #10082, .F. ) ;
#12274 = CARTESIAN_POINT ( 'NONE',  ( -9.999999999999994671, -24.16482700510257686, 16.07617750791695954 ) ) ;
#12275 = DIRECTION ( 'NONE',  ( 0.000000000000000000, 0.000000000000000000, 1.000000000000000000 ) ) ;
#12276 = ADVANCED_FACE ( 'NONE', ( #19031 ), #15803, .T. ) ;
#12277 = ORIENTED_EDGE ( 'NONE', *, *, #15152, .F. ) ;
#12278 = ADVANCED_FACE ( 'NONE', ( #6790 ), #5502, .T. ) ;
#12279 = CARTESIAN_POINT ( 'NONE',  ( -16.50457296725825174, -19.04416526290807354, 11.26757249208304046 ) ) ;
#12280 = EDGE_CURVE ( 'NONE', #13683, #5958, #10299, .T. ) ;
#12281 = EDGE_CURVE ( 'NONE', #1809, #12841, #4027, .T. ) ;
#12282 = CARTESIAN_POINT ( 'NONE',  ( -12.31951028609536536, -25.35725562635139596, 13.23632249208304223 ) ) ;
#12283 = AXIS2_PLACEMENT_3D ( 'NONE', #6335, #3575, #16820 ) ;
#12284 = DIRECTION ( 'NONE',  ( 1.000000000000000000, 0.000000000000000000, -0.000000000000000000 ) ) ;
#12285 = ORIENTED_EDGE ( 'NONE', *, *, #7715, .F. ) ;
#12286 = ORIENTED_EDGE ( 'NONE', *, *, #2222, .T. ) ;
#12287 = CARTESIAN_POINT ( 'NONE',  ( -0.9999999999999945599, -32.00000000000000000, 9.500000000000001776 ) ) ;
#12288 = DIRECTION ( 'NONE',  ( 0.000000000000000000, 1.000000000000000000, 0.000000000000000000 ) ) ;
#12289 = DIRECTION ( 'NONE',  ( -0.5000000000000034417, 0.000000000000000000, 0.8660254037844367092 ) ) ;
#12290 = LINE ( 'NONE', #13953, #10306 ) ;
#12291 = EDGE_CURVE ( 'NONE', #11714, #8784, #2458, .T. ) ;
#12292 = CARTESIAN_POINT ( 'NONE',  ( 2.499999999999996447, 65.03553390593273775, 46.44999999999999574 ) ) ;
#12293 = EDGE_CURVE ( 'NONE', #9118, #4107, #1180, .T. ) ;
#12294 = SURFACE_SIDE_STYLE ('',( #7991 ) ) ;
#12295 = LINE ( 'NONE', #12188, #8630 ) ;
#12296 = ORIENTED_EDGE ( 'NONE', *, *, #1457, .F. ) ;
#12297 = CARTESIAN_POINT ( 'NONE',  ( 32.50000000000000000, 58.00000000000000000, -35.00000000000000000 ) ) ;
#12298 = CARTESIAN_POINT ( 'NONE',  ( -18.78091578003889950, -27.53959229564985378, 18.04492750791695954 ) ) ;
#12299 = CARTESIAN_POINT ( 'NONE',  ( 4.592425496802577917E-16, 61.50000000000000000, 44.70000000218494307 ) ) ;
#12300 = CARTESIAN_POINT ( 'NONE',  ( -17.35725562635140307, -28.41254052147349185, 25.04882249208304401 ) ) ;
#12301 = CARTESIAN_POINT ( 'NONE',  ( -41.00000000000000711, 53.00000000000000711, -18.00000000000000000 ) ) ;
#12302 = CARTESIAN_POINT ( 'NONE',  ( -9.955834737091912245, -22.82508104294696594, 21.10742750791695599 ) ) ;
#12303 = FACE_OUTER_BOUND ( 'NONE', #9755, .T. ) ;
#12304 = CARTESIAN_POINT ( 'NONE',  ( -11.46040770435012490, -27.78091578003888173, 16.73242750791695954 ) ) ;
#12305 = DIRECTION ( 'NONE',  ( 0.000000000000000000, 0.7071067811865456854, 0.7071067811865494601 ) ) ;
#12306 = DIRECTION ( 'NONE',  ( -0.000000000000000000, -0.000000000000000000, -1.000000000000000000 ) ) ;
#12307 = CARTESIAN_POINT ( 'NONE',  ( 3.796994071234847710E-16, 61.93301269999999903, 48.35000000109246798 ) ) ;
#12308 = CARTESIAN_POINT ( 'NONE',  ( -15.00000000000000000, -0.000000000000000000, 37.00000000000000000 ) ) ;
#12309 = DIRECTION ( 'NONE',  ( 1.000000000000000000, 0.000000000000000000, 0.000000000000000000 ) ) ;
#12310 = EDGE_CURVE ( 'NONE', #297, #11681, #966, .T. ) ;
#12311 = FILL_AREA_STYLE ('',( #5256 ) ) ;
#12312 = CARTESIAN_POINT ( 'NONE',  ( 1.461580736456473684, 65.46158073645646880, 46.25000000109246656 ) ) ;
#12313 = CARTESIAN_POINT ( 'NONE',  ( -32.50000000000001421, 0.000000000000000000, 42.49999999999997868 ) ) ;
#12314 = EDGE_LOOP ( 'NONE', ( #7159, #6166, #15980, #4682 ) ) ;
#12315 = ORIENTED_EDGE ( 'NONE', *, *, #11372, .F. ) ;
#12316 = CARTESIAN_POINT ( 'NONE',  ( -18.35725562635138886, -30.14459132904237393, 30.29882249208304401 ) ) ;
#12317 = SURFACE_STYLE_FILL_AREA ( #16739 ) ;
#12318 = CARTESIAN_POINT ( 'NONE',  ( -10.58745947852648328, -26.35725562635138530, 7.986322492083041347 ) ) ;
#12319 = ORIENTED_EDGE ( 'NONE', *, *, #14705, .T. ) ;
#12320 = CARTESIAN_POINT ( 'NONE',  ( -12.31951028609537602, -22.64274437364854364, 26.13867750791696309 ) ) ;
#12321 = CARTESIAN_POINT ( 'NONE',  ( -41.99999999999997868, 6.000000000000005329, 51.99999999999997868 ) ) ;
#12322 = CARTESIAN_POINT ( 'NONE',  ( -12.95952864787948755, -30.95583473709188382, 19.14257249208303691 ) ) ;
#12323 = CARTESIAN_POINT ( 'NONE',  ( 2.066987300000002303, 63.14382582708705627, 46.70000000109248361 ) ) ;
#12324 = CARTESIAN_POINT ( 'NONE',  ( -1.461580736456473462, 62.53841926354353120, 45.65000000109247225 ) ) ;
#12325 = ORIENTED_EDGE ( 'NONE', *, *, #3972, .T. ) ;
#12326 = VERTEX_POINT ( 'NONE', #5317 ) ;
#12327 = CARTESIAN_POINT ( 'NONE',  ( 49.99999999999998579, 3.000000000000000000, 59.99999999999997868 ) ) ;
#12328 = CARTESIAN_POINT ( 'NONE',  ( 0.08838834764831179913, 29.68014068711925901, 56.80514068711929809 ) ) ;
#12329 = ORIENTED_EDGE ( 'NONE', *, *, #11539, .T. ) ;
#12330 = CARTESIAN_POINT ( 'NONE',  ( -0.8561741729129461742, 66.06698730000000808, 49.40000000109247225 ) ) ;
#12331 = LINE ( 'NONE', #2138, #16259 ) ;
#12332 = PLANE ( 'NONE',  #16952 ) ;
#12333 = DIRECTION ( 'NONE',  ( 1.000000000000000000, 0.000000000000000000, -7.709882115452476934E-17 ) ) ;
#12334 = PLANE ( 'NONE',  #17100 ) ;
#12335 = VERTEX_POINT ( 'NONE', #11560 ) ;
#12337 = VERTEX_POINT ( 'NONE', #18666 ) ;
#12336 = ORIENTED_EDGE ( 'NONE', *, *, #12707, .F. ) ;
#12338 = CARTESIAN_POINT ( 'NONE',  ( -9.754982604823348780, -18.99630608921234654, 31.16992750791695954 ) ) ;
#12339 =( LENGTH_UNIT ( ) NAMED_UNIT ( * ) SI_UNIT ( .MILLI., .METRE. ) );
#12340 = ORIENTED_EDGE ( 'NONE', *, *, #3536, .F. ) ;
#12341 = ORIENTED_EDGE ( 'NONE', *, *, #16580, .F. ) ;
#12342 = CARTESIAN_POINT ( 'NONE',  ( -18.04416526290808775, -23.36097942780924441, 15.64257249208304579 ) ) ;
#12343 = CARTESIAN_POINT ( 'NONE',  ( -20.00369391078762860, -18.75498260482333279, 14.10742750791695777 ) ) ;
#12344 = VECTOR ( 'NONE', #10002, 1000.000000000000000 ) ;
#12345 = CARTESIAN_POINT ( 'NONE',  ( -1.461580736456473462, 62.53841926354353120, 48.85000000109246798 ) ) ;
#12346 = DIRECTION ( 'NONE',  ( 0.000000000000000000, 0.000000000000000000, -1.000000000000000000 ) ) ;
#12347 = ORIENTED_EDGE ( 'NONE', *, *, #10982, .F. ) ;
#12348 = CARTESIAN_POINT ( 'NONE',  ( -15.63902057219076269, -20.95583473709189448, 19.79492750791695954 ) ) ;
#12349 = SURFACE_STYLE_FILL_AREA ( #6580 ) ;
#12350 = ORIENTED_EDGE ( 'NONE', *, *, #3297, .F. ) ;
#12351 = CARTESIAN_POINT ( 'NONE',  ( -41.00000000000000711, 53.00000000000000711, -18.00000000000000000 ) ) ;
#12352 = VERTEX_POINT ( 'NONE', #14615 ) ;
#12353 = DIRECTION ( 'NONE',  ( -7.304098846218135653E-17, 0.000000000000000000, 1.000000000000000000 ) ) ;
#12354 = DIRECTION ( 'NONE',  ( 1.000000000000000000, 0.000000000000000000, 0.000000000000000000 ) ) ;
#12355 = FACE_BOUND ( 'NONE', #12664, .T. ) ;
#12356 = EDGE_CURVE ( 'NONE', #16683, #1832, #17278, .T. ) ;
#12357 = CARTESIAN_POINT ( 'NONE',  ( -41.00000000000000711, 110.0000000000000000, -19.00000000000000000 ) ) ;
#12358 = CARTESIAN_POINT ( 'NONE',  ( -2.066987300000001859, 64.85617417291294373, 49.50000000109246656 ) ) ;
#12359 = ITEM_DEFINED_TRANSFORMATION ( 'NONE', 'NONE', #2036,  #1791 ) ;
#12360 = FACE_OUTER_BOUND ( 'NONE', #394, .T. ) ;
#12361 = LINE ( 'NONE', #18735, #3773 ) ;
#12362 = COLOUR_RGB ( '', 0.08235294, 0.09019608, 0.10196078) ;
#12363 = CYLINDRICAL_SURFACE ( 'NONE', #14283, 2.649999999999992806 ) ;
#12364 = AXIS2_PLACEMENT_3D ( 'NONE', #10920, #13871, #14164 ) ;
#12365 = CARTESIAN_POINT ( 'NONE',  ( 2.500000000000000000, -2.357898499370432610, 3.252606517456513302E-15 ) ) ;
#12366 = ORIENTED_EDGE ( 'NONE', *, *, #5392, .T. ) ;
#12367 = EDGE_CURVE ( 'NONE', #109, #6502, #4137, .T. ) ;
#12368 = CARTESIAN_POINT ( 'NONE',  ( -19.24771351637089367, -21.35725562635142438, 13.88867750791695954 ) ) ;
#12369 = CARTESIAN_POINT ( 'NONE',  ( -32.50000000000000000, 53.00000000000000711, -35.00000000000000000 ) ) ;
#12370 = ORIENTED_EDGE ( 'NONE', *, *, #17683, .T. ) ;
#12371 = UNCERTAINTY_MEASURE_WITH_UNIT (LENGTH_MEASURE( 1.000000000000000082E-05 ), #6446, 'distance_accuracy_value', 'NONE');
#12372 = CARTESIAN_POINT ( 'NONE',  ( -11.21908421996106320, -27.53959229564982181, 13.45507249208304223 ) ) ;
#12373 = CARTESIAN_POINT ( 'NONE',  ( -17.68048971390462754, -22.64274437364856496, 21.11132249208304401 ) ) ;
#12374 =( GEOMETRIC_REPRESENTATION_CONTEXT ( 3 ) GLOBAL_UNCERTAINTY_ASSIGNED_CONTEXT ( ( #2761 ) ) GLOBAL_UNIT_ASSIGNED_CONTEXT ( ( #4144, #17862, #10095 ) ) REPRESENTATION_CONTEXT ( 'NONE', 'WORKASPACE' ) );
#12375 = FACE_OUTER_BOUND ( 'NONE', #5757, .T. ) ;
#12376 = ORIENTED_EDGE ( 'NONE', *, *, #13319, .T. ) ;
#12377 = VECTOR ( 'NONE', #2651, 1000.000000000000000 ) ;
#12378 = CARTESIAN_POINT ( 'NONE',  ( -25.00000000000000000, 110.0000000000000000, 30.00000000000000000 ) ) ;
#12379 = ORIENTED_EDGE ( 'NONE', *, *, #5680, .T. ) ;
#12380 = CARTESIAN_POINT ( 'NONE',  ( -3.400000000000017675, 29.83102903476760659, 56.65425233947095762 ) ) ;
#12381 = LINE ( 'NONE', #10904, #18006 ) ;
#12382 = DIRECTION ( 'NONE',  ( -1.541976423090495880E-16, 0.000000000000000000, 1.000000000000000000 ) ) ;
#12383 = ADVANCED_FACE ( 'NONE', ( #4527 ), #110, .F. ) ;
#12384 = EDGE_CURVE ( 'NONE', #10477, #15869, #1585, .T. ) ;
#12385 = CARTESIAN_POINT ( 'NONE',  ( 3.796994071234847710E-16, 61.93301269999999903, 45.15000000109247225 ) ) ;
#12386 = ADVANCED_FACE ( 'NONE', ( #3047 ), #18056, .F. ) ;
#12387 = SURFACE_SIDE_STYLE ('',( #14049 ) ) ;
#12388 = CARTESIAN_POINT ( 'NONE',  ( -41.00000000000000711, 110.0000000000000000, 1.500000000000001332 ) ) ;
#12389 = VECTOR ( 'NONE', #16788, 1000.000000000000000 ) ;
#12390 = AXIS2_PLACEMENT_3D ( 'NONE', #15269, #1838, #7822 ) ;
#12391 = ORIENTED_EDGE ( 'NONE', *, *, #18936, .F. ) ;
#12392 = CARTESIAN_POINT ( 'NONE',  ( -19.95583473709191580, -22.49542703274176603, 18.91992750791694888 ) ) ;
#12393 = CARTESIAN_POINT ( 'NONE',  ( 4.592425496802577917E-16, 61.50000000000000000, 47.10000000218494165 ) ) ;
#12394 = CARTESIAN_POINT ( 'NONE',  ( -10.75228648362912232, -21.35725562635138530, 17.61132249208304401 ) ) ;
#12395 = DIRECTION ( 'NONE',  ( 0.000000000000000000, 0.7071067811865456854, 0.7071067811865493491 ) ) ;
#12396 = CARTESIAN_POINT ( 'NONE',  ( -12.64274437364855252, -28.41254052147347053, 16.95117750791695954 ) ) ;
#12397 = DIRECTION ( 'NONE',  ( -1.000000000000000000, 0.000000000000000000, 8.163404592832032733E-17 ) ) ;
#12398 = VECTOR ( 'NONE', #1734, 1000.000000000000000 ) ;
#12399 = CARTESIAN_POINT ( 'NONE',  ( -19.41254052147348830, -26.35725562635142083, 23.51367750791695954 ) ) ;
#12400 = CARTESIAN_POINT ( 'NONE',  ( 32.50000000000000000, 0.000000000000000000, -45.00000000000000000 ) ) ;
#12401 = CARTESIAN_POINT ( 'NONE',  ( -18.78091578003892792, -20.46040770435013556, 26.58007249208304401 ) ) ;
#12402 = ADVANCED_FACE ( 'NONE', ( #19130 ), #16181, .F. ) ;
#12403 = VECTOR ( 'NONE', #9635, 1000.000000000000000 ) ;
#12404 = CARTESIAN_POINT ( 'NONE',  ( 2.066987300000002303, 63.14382582708705627, 46.90000000109247225 ) ) ;
#12405 = PLANE ( 'NONE',  #14981 ) ;
#12406 = CARTESIAN_POINT ( 'NONE',  ( -1.485306817036799787, -37.50000000000000000, 7.499999999999995559 ) ) ;
#12407 = SURFACE_STYLE_USAGE ( .BOTH. , #5071 ) ;
#12408 = CARTESIAN_POINT ( 'NONE',  ( -0.8561741729129461742, 66.06698729999999387, 48.80000000109247082 ) ) ;
#12409 = LINE ( 'NONE', #361, #2075 ) ;
#12410 = ORIENTED_EDGE ( 'NONE', *, *, #15493, .F. ) ;
#12411 = ORIENTED_EDGE ( 'NONE', *, *, #17534, .F. ) ;
#12412 = CARTESIAN_POINT ( 'NONE',  ( -14.83517299489734853, -30.99999999999998224, 35.11132249208304046 ) ) ;
#12413 = AXIS2_PLACEMENT_3D ( 'NONE', #12369, #417, #10992 ) ;
#12414 = FILL_AREA_STYLE_COLOUR ( '', #12362 ) ;
#12415 = AXIS2_PLACEMENT_3D ( 'NONE', #12651, #14130, #13933 ) ;
#12416 = CARTESIAN_POINT ( 'NONE',  ( -19.95583473709190514, -25.50457296725823042, 9.955072492083040459 ) ) ;
#12417 = ORIENTED_EDGE ( 'NONE', *, *, #6177, .F. ) ;
#12418 = CARTESIAN_POINT ( 'NONE',  ( -14.36097942780923731, -27.04416526290806999, 32.91992750791696665 ) ) ;
#12419 = CARTESIAN_POINT ( 'NONE',  ( -41.00000000000000711, 53.00000000000000711, 26.50000000000000000 ) ) ;
#12420 = CARTESIAN_POINT ( 'NONE',  ( -21.95583473709189803, -26.04047135212049469, 25.70507249208304046 ) ) ;
#12421 = CARTESIAN_POINT ( 'NONE',  ( 0.8561741729129472844, 61.93301270000000613, 45.80000000109246372 ) ) ;
#12422 = CARTESIAN_POINT ( 'NONE',  ( 0.8561741729129472844, 61.93301270000000613, 47.40000000109247225 ) ) ;
#12423 = VERTEX_POINT ( 'NONE', #1385 ) ;
#12424 = EDGE_CURVE ( 'NONE', #13301, #4424, #14816, .T. ) ;
#12425 = ORIENTED_EDGE ( 'NONE', *, *, #10310, .T. ) ;
#12426 = CARTESIAN_POINT ( 'NONE',  ( -14.99999999999999645, 52.00000000000000711, 20.99999999999998224 ) ) ;
#12427 = CARTESIAN_POINT ( 'NONE',  ( 1.000000000000001998, -32.00000000000000000, 9.500000000000001776 ) ) ;
#12428 = CARTESIAN_POINT ( 'NONE',  ( -0.8561741729129466183, 61.93301270000000613, 48.90000000109247225 ) ) ;
#12429 = CARTESIAN_POINT ( 'NONE',  ( 1.300000000000000044, 0.000000000000000000, 0.000000000000000000 ) ) ;
#12430 = AXIS2_PLACEMENT_3D ( 'NONE', #9893, #795, #5307 ) ;
#12431 = CARTESIAN_POINT ( 'NONE',  ( -3.065533689247737392, -46.96461745799954457, 3.000000000000000000 ) ) ;
#12432 = EDGE_CURVE ( 'NONE', #4916, #7133, #9124, .T. ) ;
#12433 = DIRECTION ( 'NONE',  ( 0.000000000000000000, 0.000000000000000000, 1.000000000000000000 ) ) ;
#12434 = ORIENTED_EDGE ( 'NONE', *, *, #18994, .T. ) ;
#12436 = ORIENTED_EDGE ( 'NONE', *, *, #706, .T. ) ;
#12435 = ORIENTED_EDGE ( 'NONE', *, *, #7244, .T. ) ;
#12437 = CARTESIAN_POINT ( 'NONE',  ( -21.95583473709191580, -21.95952864787954084, 24.16992750791695954 ) ) ;
#12438 = PRESENTATION_STYLE_ASSIGNMENT (( #10669 ) ) ;
#12439 = ORIENTED_EDGE ( 'NONE', *, *, #3646, .F. ) ;
#12440 = ORIENTED_EDGE ( 'NONE', *, *, #866, .T. ) ;
#12441 = CARTESIAN_POINT ( 'NONE',  ( -13.64274437364857739, -21.31951028609534760, 27.67382249208304401 ) ) ;
#12442 = CARTESIAN_POINT ( 'NONE',  ( -8.044165262908075320, -26.04047135212042718, 21.54492750791695599 ) ) ;
#12443 = CARTESIAN_POINT ( 'NONE',  ( -2.066987300000001415, 64.85617417291294373, 48.70000000109247651 ) ) ;
#12444 = CARTESIAN_POINT ( 'NONE',  ( -2.492551403682565780, 31.20336399182265552, 54.92836399182263563 ) ) ;
#12445 = ORIENTED_EDGE ( 'NONE', *, *, #4554, .T. ) ;
#12446 = CARTESIAN_POINT ( 'NONE',  ( -13.64274437364856141, -26.68048971390460622, 22.20117750791696309 ) ) ;
#12447 = ORIENTED_EDGE ( 'NONE', *, *, #2832, .T. ) ;
#12448 = CARTESIAN_POINT ( 'NONE',  ( 1.753982408753060440, -45.28611686177728046, 1.500000000000000000 ) ) ;
#12449 = ORIENTED_EDGE ( 'NONE', *, *, #9387, .T. ) ;
#12450 = CYLINDRICAL_SURFACE ( 'NONE', #7568, 2.499999999999998668 ) ;
#12451 = CARTESIAN_POINT ( 'NONE',  ( 44.99999999999998579, 3.000000000000000000, -54.99999999999998579 ) ) ;
#12452 = CARTESIAN_POINT ( 'NONE',  ( 0.1249999999999895917, 31.97002704785689531, 54.16170093578840294 ) ) ;
#12453 = CARTESIAN_POINT ( 'NONE',  ( -41.00000000000000711, 53.00000000000000711, -38.50000000000000711 ) ) ;
#12454 = CARTESIAN_POINT ( 'NONE',  ( 0.8561741729129472844, 61.93301270000000613, 49.00000000109246656 ) ) ;
#12455 = CONTEXT_DEPENDENT_SHAPE_REPRESENTATION ( #5440, #15831 ) ;
#12456 = PLANE ( 'NONE',  #8055 ) ;
#12457 = LINE ( 'NONE', #18454, #14724 ) ;
#12458 = CARTESIAN_POINT ( 'NONE',  ( -1.485306817036799787, -37.50000000000000000, -3.000000000000000000 ) ) ;
#12459 = DIRECTION ( 'NONE',  ( 1.000000000000000000, 0.000000000000000000, -0.000000000000000000 ) ) ;
#12460 = VERTEX_POINT ( 'NONE', #8923 ) ;
#12461 = CARTESIAN_POINT ( 'NONE',  ( -18.78091578003889950, -27.53959229564985378, 28.54492750791695954 ) ) ;
#12462 = LINE ( 'NONE', #323, #2086 ) ;
#12463 = ORIENTED_EDGE ( 'NONE', *, *, #2473, .T. ) ;
#12464 = CARTESIAN_POINT ( 'NONE',  ( -20.04416526290809131, -22.82508104294699791, 31.39257249208304046 ) ) ;
#12465 = CARTESIAN_POINT ( 'NONE',  ( -11.99999999999999289, -23.83517299489735564, 23.29882249208304046 ) ) ;
#12466 = EDGE_LOOP ( 'NONE', ( #2959, #10169, #15406, #15981 ) ) ;
#12467 = LINE ( 'NONE', #18470, #8736 ) ;
#12468 = ORIENTED_EDGE ( 'NONE', *, *, #3737, .F. ) ;
#12469 = LINE ( 'NONE', #18472, #11553 ) ;
#12470 = EDGE_CURVE ( 'NONE', #6094, #14223, #7357, .T. ) ;
#12471 = EDGE_CURVE ( 'NONE', #9436, #17811, #11757, .T. ) ;
#12472 = DIRECTION ( 'NONE',  ( 0.000000000000000000, 0.000000000000000000, -1.000000000000000000 ) ) ;
#12473 = VECTOR ( 'NONE', #3489, 1000.000000000000000 ) ;
#12474 = CARTESIAN_POINT ( 'NONE',  ( -1.530808498934192803E-16, 66.50000000000000000, 45.90000000218494591 ) ) ;
#12475 = DIRECTION ( 'NONE',  ( -0.7071067811865414665, 0.5000000000000057732, -0.5000000000000028866 ) ) ;
#12476 = ADVANCED_FACE ( 'NONE', ( #11663 ), #14711, .F. ) ;
#12477 = FACE_OUTER_BOUND ( 'NONE', #17933, .T. ) ;
#12478 = FACE_OUTER_BOUND ( 'NONE', #242, .T. ) ;
#12480 = EDGE_CURVE ( 'NONE', #11212, #18570, #15111, .T. ) ;
#12479 = CARTESIAN_POINT ( 'NONE',  ( 0.000000000000000000, 0.000000000000000000, 3.000000000000000000 ) ) ;
#12481 = DIRECTION ( 'NONE',  ( -0.000000000000000000, -0.000000000000000000, -1.000000000000000000 ) ) ;
#12482 = EDGE_LOOP ( 'NONE', ( #17523, #4065, #5031, #6944 ) ) ;
#12483 = CIRCLE ( 'NONE', #6554, 5.800000000000007816 ) ;
#12484 = CARTESIAN_POINT ( 'NONE',  ( -20.04416526290808065, -25.17491895705300209, 18.48242750791695954 ) ) ;
#12485 = CARTESIAN_POINT ( 'NONE',  ( 1.035533905932738197, 66.50000000000000000, 47.45000000218495018 ) ) ;
#12486 = EDGE_CURVE ( 'NONE', #5657, #9274, #17857, .T. ) ;
#12487 = CARTESIAN_POINT ( 'NONE',  ( -15.16482700510263371, -18.99999999999997868, 16.73632249208304401 ) ) ;
#12488 = B_SPLINE_CURVE_WITH_KNOTS ( 'NONE', 3,
 ( #11636, #4402, #1157, #4301 ),
 .UNSPECIFIED., .F., .F.,
 ( 4, 4 ),
 ( 0.000000000000000000, 1.000000000000000000 ),
 .UNSPECIFIED. ) ;
#12489 = CARTESIAN_POINT ( 'NONE',  ( -24.00000000000000000, 53.00000000000000711, 27.50000000000000000 ) ) ;
#12490 = CARTESIAN_POINT ( 'NONE',  ( -10.58745947852649927, -21.64274437364853654, 15.63867750791695777 ) ) ;
#12491 = CARTESIAN_POINT ( 'NONE',  ( 2.315774708385922587, 27.80336399182260720, 58.32836399182267684 ) ) ;
#12493 = CARTESIAN_POINT ( 'NONE',  ( -11.21908421996108984, -20.46040770435011069, 36.41992750791696665 ) ) ;
#12492 = CONICAL_SURFACE ( 'NONE', #14669, 1.280000000000000027, 1.047197551196593857 ) ;
#12494 = CARTESIAN_POINT ( 'NONE',  ( 4.012830983233625304, 26.60336399182260791, 59.52836399182266547 ) ) ;
#12495 = CARTESIAN_POINT ( 'NONE',  ( -10.58745947852648328, -26.35725562635138530, 28.98632249208304401 ) ) ;
#12496 = ADVANCED_FACE ( 'NONE', ( #2946 ), #14915, .F. ) ;
#12497 = CARTESIAN_POINT ( 'NONE',  ( -0.8561741729129461742, 66.06698729999999387, 48.00000000109246656 ) ) ;
#12498 = PLANE ( 'NONE',  #18439 ) ;
#12499 = CARTESIAN_POINT ( 'NONE',  ( 7.500000000000005329, -38.00000000000000000, 12.50000000000000000 ) ) ;
#12500 = VECTOR ( 'NONE', #3022, 1000.000000000000000 ) ;
#12501 =( NAMED_UNIT ( * ) PLANE_ANGLE_UNIT ( ) SI_UNIT ( $, .RADIAN. ) );
#12502 = CARTESIAN_POINT ( 'NONE',  ( 3.796994071234847710E-16, 61.93301269999999903, 48.35000000109246798 ) ) ;
#12503 = DIRECTION ( 'NONE',  ( -0.000000000000000000, -1.000000000000000000, -0.000000000000000000 ) ) ;
#12504 = VERTEX_POINT ( 'NONE', #17756 ) ;
#12505 = ORIENTED_EDGE ( 'NONE', *, *, #18977, .T. ) ;
#12506 = CARTESIAN_POINT ( 'NONE',  ( -8.855408670957602979, -27.35725562635137820, 28.98632249208304401 ) ) ;
#12507 = VECTOR ( 'NONE', #10873, 1000.000000000000000 ) ;
#12508 = EDGE_CURVE ( 'NONE', #11681, #17737, #7160, .T. ) ;
#12509 = CARTESIAN_POINT ( 'NONE',  ( -16.50457296725825174, -19.04416526290807354, 16.51757249208304046 ) ) ;
#12511 = ORIENTED_EDGE ( 'NONE', *, *, #15879, .T. ) ;
#12510 = EDGE_CURVE ( 'NONE', #3632, #9208, #4326, .T. ) ;
#12512 = CARTESIAN_POINT ( 'NONE',  ( -12.04416526290807887, -24.96867458239596260, 26.79492750791695954 ) ) ;
#12513 = CARTESIAN_POINT ( 'NONE',  ( -47.00000000000002132, 6.000000000000000000, -57.00000000000001421 ) ) ;
#12514 = CARTESIAN_POINT ( 'NONE',  ( -7.955834737091903364, -25.71081734191518464, 18.26757249208304046 ) ) ;
#12515 = VECTOR ( 'NONE', #18956, 1000.000000000000000 ) ;
#12516 = CARTESIAN_POINT ( 'NONE',  ( -0.8561741729129465073, 61.93301270000000613, 47.30000000109247082 ) ) ;
#12517 = CARTESIAN_POINT ( 'NONE',  ( -1.461580736456473906, 65.46158073645646880, 44.65000000109246514 ) ) ;
#12518 = ORIENTED_EDGE ( 'NONE', *, *, #15123, .F. ) ;
#12519 = ORIENTED_EDGE ( 'NONE', *, *, #4697, .T. ) ;
#12520 = ADVANCED_FACE ( 'NONE', ( #10 ), #15008, .F. ) ;
#12521 = CARTESIAN_POINT ( 'NONE',  ( 24.00000000000000000, 0.000000000000000000, -67.72004514666936359 ) ) ;
#12522 = LINE ( 'NONE', #16751, #16359 ) ;
#12523 = AXIS2_PLACEMENT_3D ( 'NONE', #13719, #4, #11958 ) ;
#12524 = CARTESIAN_POINT ( 'NONE',  ( 2.066987300000001415, 64.85617417291294373, 49.20000000109247651 ) ) ;
#12525 = LINE ( 'NONE', #11048, #12190 ) ;
#12526 = FACE_OUTER_BOUND ( 'NONE', #19087, .T. ) ;
#12527 = VECTOR ( 'NONE', #4925, 1000.000000000000114 ) ;
#12528 = CARTESIAN_POINT ( 'NONE',  ( -32.50000000000001421, -6.000000000000000000, 44.99999999999997868 ) ) ;
#12529 = DIRECTION ( 'NONE',  ( -2.973811673103096679E-16, 0.000000000000000000, 1.000000000000000000 ) ) ;
#12530 = EDGE_CURVE ( 'NONE', #12139, #9017, #7518, .T. ) ;
#12531 = ORIENTED_EDGE ( 'NONE', *, *, #11906, .F. ) ;
#12532 = ORIENTED_EDGE ( 'NONE', *, *, #4394, .F. ) ;
#12533 = CARTESIAN_POINT ( 'NONE',  ( -9.996306089212364299, -29.24501739517662813, 32.48242750791695244 ) ) ;
#12534 = LINE ( 'NONE', #16862, #14608 ) ;
#12535 = VERTEX_POINT ( 'NONE', #9603 ) ;
#12537 = VERTEX_POINT ( 'NONE', #5116 ) ;
#12536 = ORIENTED_EDGE ( 'NONE', *, *, #11143, .T. ) ;
#12538 = CARTESIAN_POINT ( 'NONE',  ( -12.31951028609536536, -25.35725562635139596, 34.23632249208304756 ) ) ;
#12539 = CARTESIAN_POINT ( 'NONE',  ( -9.996306089212364299, -29.24501739517662813, 21.98242750791695599 ) ) ;
#12540 = VECTOR ( 'NONE', #18154, 1000.000000000000000 ) ;
#12541 = LINE ( 'NONE', #9687, #8208 ) ;
#12542 = DIRECTION ( 'NONE',  ( 0.000000000000000000, 0.000000000000000000, 1.000000000000000000 ) ) ;
#12543 = PLANE ( 'NONE',  #5026 ) ;
#12544 = EDGE_LOOP ( 'NONE', ( #16860, #15689 ) ) ;
#12545 = CARTESIAN_POINT ( 'NONE',  ( -12.48433729119798130, -25.64274437364855075, 27.01367750791695954 ) ) ;
#12546 = VECTOR ( 'NONE', #1666, 1000.000000000000000 ) ;
#12547 = SURFACE_STYLE_USAGE ( .BOTH. , #8145 ) ;
#12548 = ORIENTED_EDGE ( 'NONE', *, *, #7076, .T. ) ;
#12549 = DIRECTION ( 'NONE',  ( 1.000000000000000000, -0.000000000000000000, -0.000000000000000000 ) ) ;
#12550 = ORIENTED_EDGE ( 'NONE', *, *, #7198, .F. ) ;
#12551 = CARTESIAN_POINT ( 'NONE',  ( -41.00000000000000711, 110.0000000000000000, -25.50000000000000000 ) ) ;
#12552 = PRODUCT_DEFINITION ( 'UNKNOWN', '', #484, #16890 ) ;
#12553 = CARTESIAN_POINT ( 'NONE',  ( 0.000000000000000000, 0.000000000000000000, 0.000000000000000000 ) ) ;
#12554 = DIRECTION ( 'NONE',  ( 0.000000000000000000, 1.000000000000000000, 0.000000000000000000 ) ) ;
#12555 = FACE_OUTER_BOUND ( 'NONE', #17425, .T. ) ;
#12556 = CARTESIAN_POINT ( 'NONE',  ( -2.066987300000001415, 64.00000000000000000, 47.95000000109246940 ) ) ;
#12557 = ITEM_DEFINED_TRANSFORMATION ( 'NONE', 'NONE', #3917,  #1791 ) ;
#12558 = COLOUR_RGB ( '', 0.31764706, 0.68627451, 0.89019608) ;
#12559 = CARTESIAN_POINT ( 'NONE',  ( 0.8561741729129460632, 66.06698730000000808, 48.70000000109247651 ) ) ;
#12560 = DIRECTION ( 'NONE',  ( -1.000000000000000000, 2.720046410331633524E-15, -2.220446049250313081E-15 ) ) ;
#12561 = VECTOR ( 'NONE', #11469, 1000.000000000000000 ) ;
#12562 = PLANE ( 'NONE',  #1467 ) ;
#12563 = CARTESIAN_POINT ( 'NONE',  ( 2.161944888285726840, 65.13351296672139767, 44.99999999999997868 ) ) ;
#12564 = EDGE_CURVE ( 'NONE', #13301, #1710, #15209, .T. ) ;
#12565 = ORIENTED_EDGE ( 'NONE', *, *, #6402, .T. ) ;
#12566 = CARTESIAN_POINT ( 'NONE',  ( -19.95583473709191580, -22.49542703274176603, 34.66992750791694533 ) ) ;
#12567 = VECTOR ( 'NONE', #10861, 1000.000000000000000 ) ;
#12568 = CARTESIAN_POINT ( 'NONE',  ( -25.00000000000000711, 110.0000000000000000, 0.5000000000000004441 ) ) ;
#12569 = VERTEX_POINT ( 'NONE', #1681 ) ;
#12570 = CARTESIAN_POINT ( 'NONE',  ( -11.46040770435014977, -20.21908421996103655, 38.39257249208301914 ) ) ;
#12571 = VECTOR ( 'NONE', #13895, 1000.000000000000000 ) ;
#12572 = CARTESIAN_POINT ( 'NONE',  ( -15.96867458239599635, -21.04416526290806999, 37.51757249208305467 ) ) ;
#12573 = LINE ( 'NONE', #5036, #16283 ) ;
#12574 = VERTEX_POINT ( 'NONE', #12260 ) ;
#12575 = VECTOR ( 'NONE', #19138, 1000.000000000000000 ) ;
#12576 = DIRECTION ( 'NONE',  ( 0.000000000000000000, 0.000000000000000000, -1.000000000000000000 ) ) ;
#12577 = ORIENTED_EDGE ( 'NONE', *, *, #4635, .F. ) ;
#12578 = DIRECTION ( 'NONE',  ( 0.000000000000000000, -0.5000000000000013323, -0.8660254037844378194 ) ) ;
#12579 = CARTESIAN_POINT ( 'NONE',  ( -1.040834085586084257E-14, 27.62132034355962773, 54.62132034355965260 ) ) ;
#12580 = AXIS2_PLACEMENT_3D ( 'NONE', #15690, #7041, #11534 ) ;
#12581 = LINE ( 'NONE', #3753, #3477 ) ;
#12582 = DIRECTION ( 'NONE',  ( 0.000000000000000000, 0.7071067811865456854, 0.7071067811865493491 ) ) ;
#12583 =( NAMED_UNIT ( * ) SI_UNIT ( $, .STERADIAN. ) SOLID_ANGLE_UNIT ( ) );
#12584 = CARTESIAN_POINT ( 'NONE',  ( -41.00000000000000711, 110.0000000000000000, -30.99999999999999645 ) ) ;
#12585 = DIRECTION ( 'NONE',  ( 1.000000000000000000, 0.000000000000000000, -0.000000000000000000 ) ) ;
#12586 = UNCERTAINTY_MEASURE_WITH_UNIT (LENGTH_MEASURE( 1.000000000000000082E-05 ), #3654, 'distance_accuracy_value', 'NONE');
#12587 = EDGE_LOOP ( 'NONE', ( #6777, #1191, #2035, #17424 ) ) ;
#12588 = AXIS2_PLACEMENT_3D ( 'NONE', #16151, #8693, #1254 ) ;
#12589 = CARTESIAN_POINT ( 'NONE',  ( -10.04416526290807710, -25.50457296725819489, 26.79492750791695954 ) ) ;
#12590 = CARTESIAN_POINT ( 'NONE',  ( 1.035533905932739751, 61.50000000000000000, 46.35000000218493454 ) ) ;
#12591 = CARTESIAN_POINT ( 'NONE',  ( -20.04416526290809131, -22.82508104294699791, 26.14257249208303691 ) ) ;
#12592 = DIRECTION ( 'NONE',  ( 0.000000000000000000, 0.7071067811865493491, -0.7071067811865456854 ) ) ;
#12593 = CARTESIAN_POINT ( 'NONE',  ( -17.35725562635144215, -19.58745947852648683, 19.57617750791695954 ) ) ;
#12594 = ADVANCED_FACE ( 'NONE', ( #7658 ), #16776, .F. ) ;
#12595 = CARTESIAN_POINT ( 'NONE',  ( -19.99999999999999645, 0.000000000000000000, 1.500000000000000000 ) ) ;
#12596 = CARTESIAN_POINT ( 'NONE',  ( -11.21908421996108984, -20.46040770435011069, 25.91992750791695244 ) ) ;
#12597 = DIRECTION ( 'NONE',  ( 0.000000000000000000, 0.000000000000000000, -1.000000000000000000 ) ) ;
#12598 = CARTESIAN_POINT ( 'NONE',  ( -17.35725562635140307, -28.41254052147349185, 25.04882249208304401 ) ) ;
#12599 = CARTESIAN_POINT ( 'NONE',  ( -1.265664690411616068E-16, 66.06698730000000808, 44.75000000109247367 ) ) ;
#12600 = DIRECTION ( 'NONE',  ( -1.000000000000000000, -8.673617379884027583E-16, 0.000000000000000000 ) ) ;
#12601 = CARTESIAN_POINT ( 'NONE',  ( -2.500000000000003109, 65.03553390593272354, 48.45000000218494307 ) ) ;
#12602 = CARTESIAN_POINT ( 'NONE',  ( 0.8561741729129472844, 61.93301270000000613, 49.20000000109247651 ) ) ;
#12603 = CARTESIAN_POINT ( 'NONE',  ( 0.2500000000000002220, 0.000000000000000000, 0.000000000000000000 ) ) ;
#12604 = CLOSED_SHELL ( 'NONE', ( #6160, #19219, #15941, #17210, #14308 ) ) ;
#12605 = ORIENTED_EDGE ( 'NONE', *, *, #6915, .T. ) ;
#12606 = CARTESIAN_POINT ( 'NONE',  ( -13.28918265808478694, -16.95583473709189093, 32.70507249208304756 ) ) ;
#12607 = ADVANCED_FACE ( 'NONE', ( #9409 ), #16873, .T. ) ;
#12608 = CARTESIAN_POINT ( 'NONE',  ( 0.8561741729129471734, 61.93301270000000613, 45.00000000109247367 ) ) ;
#12609 = CARTESIAN_POINT ( 'NONE',  ( -17.51566270880201159, -22.35725562635141728, 24.38867750791696665 ) ) ;
#12610 = FACE_OUTER_BOUND ( 'NONE', #3306, .T. ) ;
#12611 = CARTESIAN_POINT ( 'NONE',  ( -18.35725562635138886, -30.14459132904237393, 25.04882249208303691 ) ) ;
#12612 = CARTESIAN_POINT ( 'NONE',  ( 2.066987300000001859, 64.85617417291294373, 47.60000000109246798 ) ) ;
#12613 = VERTEX_POINT ( 'NONE', #11071 ) ;
#12614 = VERTEX_POINT ( 'NONE', #7862 ) ;
#12615 = FACE_OUTER_BOUND ( 'NONE', #287, .T. ) ;
#12616 = LINE ( 'NONE', #15276, #16327 ) ;
#12617 = CARTESIAN_POINT ( 'NONE',  ( 1.461580736456473906, 62.53841926354353120, 47.45000000109246940 ) ) ;
#12618 = CARTESIAN_POINT ( 'NONE',  ( -2.500000000000001776, 64.00000000000000000, 49.99999999999999289 ) ) ;
#12619 = CARTESIAN_POINT ( 'NONE',  ( 24.99999999999999289, 0.000000000000000000, -47.50000000000002132 ) ) ;
#12620 = EDGE_CURVE ( 'NONE', #13243, #13384, #5954, .T. ) ;
#12621 = EDGE_CURVE ( 'NONE', #4916, #14697, #9314, .T. ) ;
#12622 = LINE ( 'NONE', #6463, #12852 ) ;
#12623 = EDGE_CURVE ( 'NONE', #9541, #9159, #16977, .T. ) ;
#12624 = DIRECTION ( 'NONE',  ( -1.000000000000000000, 0.000000000000000000, -9.251858538542970348E-17 ) ) ;
#12625 = ORIENTED_EDGE ( 'NONE', *, *, #1919, .T. ) ;
#12626 = VERTEX_POINT ( 'NONE', #18349 ) ;
#12627 = CARTESIAN_POINT ( 'NONE',  ( -21.99999999999999289, -23.83517299489739116, 34.45117750791695954 ) ) ;
#12628 = VERTEX_POINT ( 'NONE', #13920 ) ;
#12630 = VERTEX_POINT ( 'NONE', #13624 ) ;
#12629 = ORIENTED_EDGE ( 'NONE', *, *, #8564, .F. ) ;
#12631 = CARTESIAN_POINT ( 'NONE',  ( -16.35725562635141372, -26.68048971390461332, 25.04882249208304401 ) ) ;
#12632 = CARTESIAN_POINT ( 'NONE',  ( -18.64274437364853654, -29.97976432393976509, 12.57617750791695599 ) ) ;
#12633 = FACE_BOUND ( 'NONE', #8708, .T. ) ;
#12634 = CARTESIAN_POINT ( 'NONE',  ( -1.035533905932738641, 66.50000000000000000, 46.75000000218494733 ) ) ;
#12635 = LINE ( 'NONE', #12444, #3765 ) ;
#12636 = VERTEX_POINT ( 'NONE', #588 ) ;
#12637 = CARTESIAN_POINT ( 'NONE',  ( -11.99999999999999289, -24.16482700510258752, 26.57617750791696309 ) ) ;
#12638 = DIRECTION ( 'NONE',  ( -0.000000000000000000, 1.000000000000000000, -0.000000000000000000 ) ) ;
#12639 = ORIENTED_EDGE ( 'NONE', *, *, #2549, .T. ) ;
#12640 = LINE ( 'NONE', #8147, #11892 ) ;
#12641 = EDGE_LOOP ( 'NONE', ( #11729, #12511 ) ) ;
#12642 = LINE ( 'NONE', #18447, #18835 ) ;
#12643 = ADVANCED_FACE ( 'NONE', ( #1973 ), #4390, .T. ) ;
#12644 = EDGE_CURVE ( 'NONE', #18999, #6640, #304, .T. ) ;
#12645 = DIRECTION ( 'NONE',  ( -1.000000000000000000, 0.000000000000000000, -0.000000000000000000 ) ) ;
#12646 = CARTESIAN_POINT ( 'NONE',  ( 44.99999999999997158, 3.000000000000000000, 55.00000000000000000 ) ) ;
#12647 = CARTESIAN_POINT ( 'NONE',  ( 1.461580736456473906, 62.53841926354353120, 47.45000000109246940 ) ) ;
#12648 = CARTESIAN_POINT ( 'NONE',  ( -2.066987300000000971, 63.14382582708704916, 47.40000000109247225 ) ) ;
#12649 = DIRECTION ( 'NONE',  ( 0.000000000000000000, 0.000000000000000000, 1.000000000000000000 ) ) ;
#12650 =( BOUNDED_CURVE ( )  B_SPLINE_CURVE ( 2, ( #139, #2779, #8757, #12186, #17098, #11101, #531, #12292, #18477 ),
 .UNSPECIFIED., .F., .F. ) 
 B_SPLINE_CURVE_WITH_KNOTS ( ( 3, 2, 2, 2, 3 ),
 ( 0.5714285714285713969, 0.5892857142857143016, 0.6071428571428569843, 0.6249999999999998890, 0.6428571428571427937 ),
 .UNSPECIFIED. ) 
 CURVE ( )  GEOMETRIC_REPRESENTATION_ITEM ( )  RATIONAL_B_SPLINE_CURVE ( ( 1.000000000000000000, 0.9238795325112867385, 1.000000000000000000, 0.9238795325112867385, 1.000000000000000000, 0.9238795325112867385, 1.000000000000000000, 0.9238795325112871826, 0.9999999999999995559 ) ) 
 REPRESENTATION_ITEM ( '' )  );
#12651 = CARTESIAN_POINT ( 'NONE',  ( 32.50000000000000000, 52.00000000000000711, -35.00000000000000000 ) ) ;
#12652 = CARTESIAN_POINT ( 'NONE',  ( 2.336476004967284137, 64.40336002165571472, 44.99999999999997868 ) ) ;
#12653 = VERTEX_POINT ( 'NONE', #10685 ) ;
#12654 = CARTESIAN_POINT ( 'NONE',  ( -17.35725562635144215, -19.58745947852648683, 35.32617750791695954 ) ) ;
#12655 = CARTESIAN_POINT ( 'NONE',  ( -41.00000000000000711, 53.00000000000000711, -12.50000000000000000 ) ) ;
#12656 = EDGE_LOOP ( 'NONE', ( #4467, #5192, #13317 ) ) ;
#12657 = MECHANICAL_DESIGN_GEOMETRIC_PRESENTATION_REPRESENTATION (  '', ( #6416 ), #10767 ) ;
#12658 = CARTESIAN_POINT ( 'NONE',  ( -12.64274437364858628, -19.58745947852646552, 27.67382249208304046 ) ) ;
#12659 = DIRECTION ( 'NONE',  ( -0.000000000000000000, -0.000000000000000000, -1.000000000000000000 ) ) ;
#12660 = CARTESIAN_POINT ( 'NONE',  ( -17.07549068051208963, -26.31681416490115311, 30.51757249208304756 ) ) ;
#12661 = LINE ( 'NONE', #6605, #11579 ) ;
#12662 = ORIENTED_EDGE ( 'NONE', *, *, #10181, .F. ) ;
#12663 = FACE_OUTER_BOUND ( 'NONE', #1375, .T. ) ;
#12664 = EDGE_LOOP ( 'NONE', ( #16097, #18290 ) ) ;
#12665 = EDGE_CURVE ( 'NONE', #72, #18276, #3538, .T. ) ;
#12666 = CARTESIAN_POINT ( 'NONE',  ( -2.500000000000006661, 65.03553390593272354, 45.25000000218494733 ) ) ;
#12667 = LINE ( 'NONE', #6414, #9544 ) ;
#12668 =( GEOMETRIC_REPRESENTATION_CONTEXT ( 3 ) GLOBAL_UNCERTAINTY_ASSIGNED_CONTEXT ( ( #12371 ) ) GLOBAL_UNIT_ASSIGNED_CONTEXT ( ( #6446, #4881, #13786 ) ) REPRESENTATION_CONTEXT ( 'NONE', 'WORKASPACE' ) );
#12669 = CARTESIAN_POINT ( 'NONE',  ( -2.500000000000011546, 65.03553390593272354, 46.05000000218494449 ) ) ;
#12670 = DIRECTION ( 'NONE',  ( 1.000000000000000000, -0.000000000000000000, -0.000000000000000000 ) ) ;
#12671 = DIRECTION ( 'NONE',  ( 0.000000000000000000, -1.000000000000000000, 0.000000000000000000 ) ) ;
#12672 = DIRECTION ( 'NONE',  ( 1.000000000000000000, 0.000000000000000000, 0.000000000000000000 ) ) ;
#12673 = CARTESIAN_POINT ( 'NONE',  ( -13.25000000000000178, -35.50000000000000000, 5.500000000000000000 ) ) ;
#12674 = ORIENTED_EDGE ( 'NONE', *, *, #6336, .T. ) ;
#12675 = LINE ( 'NONE', #1470, #13958 ) ;
#12676 = CARTESIAN_POINT ( 'NONE',  ( -18.78091578003889950, -27.53959229564985378, 33.79492750791696665 ) ) ;
#12677 = AXIS2_PLACEMENT_3D ( 'NONE', #9319, #3249, #1979 ) ;
#12678 = CARTESIAN_POINT ( 'NONE',  ( -2.066987300000001415, 63.14382582708705627, 47.20000000109248361 ) ) ;
#12679 = CARTESIAN_POINT ( 'NONE',  ( -13.82508104294702100, -18.95583473709188382, 27.45507249208304046 ) ) ;
#12680 = PLANE ( 'NONE',  #7824 ) ;
#12681 = CARTESIAN_POINT ( 'NONE',  ( -19.95583473709191580, -22.49542703274176603, 29.41992750791695599 ) ) ;
#12682 = CARTESIAN_POINT ( 'NONE',  ( 49.99999999999998579, 17.99999999999993250, 59.99999999999997868 ) ) ;
#12683 = CARTESIAN_POINT ( 'NONE',  ( -17.35725562635144215, -19.58745947852648683, 30.07617750791695599 ) ) ;
#12684 = DIRECTION ( 'NONE',  ( 1.000000000000000000, -0.000000000000000000, -0.000000000000000000 ) ) ;
#12685 = CARTESIAN_POINT ( 'NONE',  ( -17.35725562635140307, -28.41254052147349185, 19.79882249208304046 ) ) ;
#12686 = CARTESIAN_POINT ( 'NONE',  ( -2.500000000000001776, 64.00000000000000000, 49.19999999999999574 ) ) ;
#12687 = CARTESIAN_POINT ( 'NONE',  ( -3.155775640247338920, -41.39960408384398249, 3.000000000000000000 ) ) ;
#12688 = CARTESIAN_POINT ( 'NONE',  ( 7.500000000000005329, -26.00000000000000000, 4.500000000000000888 ) ) ;
#12689 = VECTOR ( 'NONE', #14352, 1000.000000000000000 ) ;
#12690 = LINE ( 'NONE', #6636, #12731 ) ;
#12691 = CARTESIAN_POINT ( 'NONE',  ( 2.500000000000001776, 64.00000000000000000, 48.79999999999999716 ) ) ;
#12692 = CARTESIAN_POINT ( 'NONE',  ( -41.00000000000000711, 110.0000000000000000, -6.000000000000001776 ) ) ;
#12693 = ORIENTED_EDGE ( 'NONE', *, *, #5992, .T. ) ;
#12694 = CARTESIAN_POINT ( 'NONE',  ( -3.065533689247737392, -45.28611686177728046, 3.000000000000000000 ) ) ;
#12695 = CARTESIAN_POINT ( 'NONE',  ( -14.03132541760401786, -21.04416526290806289, 25.48242750791696309 ) ) ;
#12696 = APPLICATION_CONTEXT ( 'automotive_design' ) ;
#12697 = CARTESIAN_POINT ( 'NONE',  ( -41.00000000000000711, 110.0000000000000000, -18.00000000000000000 ) ) ;
#12698 = CARTESIAN_POINT ( 'NONE',  ( -9.020235676060250896, -20.35725562635137820, 28.11132249208304046 ) ) ;
#12699 = AXIS2_PLACEMENT_3D ( 'NONE', #17508, #13191, #17610 ) ;
#12700 = VECTOR ( 'NONE', #3871, 1000.000000000000000 ) ;
#12701 = CARTESIAN_POINT ( 'NONE',  ( 2.066987300000001859, 64.85617417291294373, 46.80000000109246372 ) ) ;
#12702 = ORIENTED_EDGE ( 'NONE', *, *, #1423, .T. ) ;
#12703 = CARTESIAN_POINT ( 'NONE',  ( -4.000000000000001776, 67.00000000000000000, 30.00000000000000000 ) ) ;
#12704 = CARTESIAN_POINT ( 'NONE',  ( 46.99999999999998579, 115.0000000000000000, 59.99999999999997868 ) ) ;
#12705 = CARTESIAN_POINT ( 'NONE',  ( 0.8561741729129471734, 61.93301270000000613, 46.60000000109246798 ) ) ;
#12706 = CARTESIAN_POINT ( 'NONE',  ( -1.040834085586084257E-14, 34.55096679918779756, 51.93431457505078441 ) ) ;
#12707 = EDGE_CURVE ( 'NONE', #17051, #8350, #18152, .T. ) ;
#12708 = EDGE_CURVE ( 'NONE', #19128, #13505, #2065, .T. ) ;
#12709 = PLANE ( 'NONE',  #7546 ) ;
#12710 = CARTESIAN_POINT ( 'NONE',  ( 1.035533905932739751, 61.50000000000000000, 48.64999999999999858 ) ) ;
#12711 = VECTOR ( 'NONE', #8072, 1000.000000000000000 ) ;
#12712 = ADVANCED_BREP_SHAPE_REPRESENTATION ( '', ( #16836, #1791 ), #2725 ) ;
#12713 = LINE ( 'NONE', #6831, #15532 ) ;
#12714 = ORIENTED_EDGE ( 'NONE', *, *, #11313, .T. ) ;
#12715 = ORIENTED_EDGE ( 'NONE', *, *, #13297, .F. ) ;
#12716 = CARTESIAN_POINT ( 'NONE',  ( -7.999999999999996447, -24.16482700510256976, 31.82617750791695954 ) ) ;
#12717 = ORIENTED_EDGE ( 'NONE', *, *, #5642, .T. ) ;
#12719 = ORIENTED_EDGE ( 'NONE', *, *, #18839, .T. ) ;
#12718 = ORIENTED_EDGE ( 'NONE', *, *, #19065, .F. ) ;
#12720 = CARTESIAN_POINT ( 'NONE',  ( -17.68048971390462754, -22.64274437364856496, 31.61132249208304401 ) ) ;
#12721 = CARTESIAN_POINT ( 'NONE',  ( -11.64274437364854187, -30.14459132904234195, 37.95117750791695244 ) ) ;
#12722 = EDGE_CURVE ( 'NONE', #964, #7747, #211, .T. ) ;
#12723 = CARTESIAN_POINT ( 'NONE',  ( 2.500000000000006661, 65.03553390593272354, 47.24999999999998579 ) ) ;
#12724 = CARTESIAN_POINT ( 'NONE',  ( -2.500000000000001776, 65.03553390593273775, 48.45000000218495018 ) ) ;
#12725 = DIRECTION ( 'NONE',  ( 0.000000000000000000, -1.000000000000000000, -0.000000000000000000 ) ) ;
#12726 = ORIENTED_EDGE ( 'NONE', *, *, #11376, .T. ) ;
#12727 = EDGE_CURVE ( 'NONE', #4122, #5104, #16376, .T. ) ;
#12728 = CARTESIAN_POINT ( 'NONE',  ( -12.92450931948788906, -26.31681416490114245, 27.23242750791697020 ) ) ;
#12729 = DIRECTION ( 'NONE',  ( 0.000000000000000000, -1.000000000000000000, -0.000000000000000000 ) ) ;
#12730 = ORIENTED_EDGE ( 'NONE', *, *, #17408, .T. ) ;
#12731 = VECTOR ( 'NONE', #14171, 1000.000000000000000 ) ;
#12732 = CARTESIAN_POINT ( 'NONE',  ( -10.00000000000000000, 35.00000000000000000, 0.000000000000000000 ) ) ;
#12733 = ORIENTED_EDGE ( 'NONE', *, *, #16815, .T. ) ;
#12734 = FACE_OUTER_BOUND ( 'NONE', #167, .T. ) ;
#12735 = CARTESIAN_POINT ( 'NONE',  ( -11.25000000000000178, -35.50000000000000000, 1.500000000000000000 ) ) ;
#12736 = LINE ( 'NONE', #783, #15014 ) ;
#12737 = CARTESIAN_POINT ( 'NONE',  ( -0.8561741729129461742, 66.06698729999999387, 45.40000000109246514 ) ) ;
#12738 = CARTESIAN_POINT ( 'NONE',  ( -1.461580736456473462, 62.53841926354353120, 48.25000000109246656 ) ) ;
#12739 = DIRECTION ( 'NONE',  ( 0.000000000000000000, 0.000000000000000000, -1.000000000000000000 ) ) ;
#12740 = DIRECTION ( 'NONE',  ( 1.000000000000000000, 0.000000000000000000, 0.000000000000000000 ) ) ;
#12741 = CARTESIAN_POINT ( 'NONE',  ( 0.1249999999999895917, 25.46464466094064250, 60.66708332270462734 ) ) ;
#12742 = ORIENTED_EDGE ( 'NONE', *, *, #4115, .T. ) ;
#12743 = VERTEX_POINT ( 'NONE', #12351 ) ;
#12744 = CARTESIAN_POINT ( 'NONE',  ( -10.04416526290807710, -25.50457296725819489, 32.04492750791695954 ) ) ;
#12745 =( GEOMETRIC_REPRESENTATION_CONTEXT ( 3 ) GLOBAL_UNCERTAINTY_ASSIGNED_CONTEXT ( ( #3762 ) ) GLOBAL_UNIT_ASSIGNED_CONTEXT ( ( #3707, #680, #14198 ) ) REPRESENTATION_CONTEXT ( 'NONE', 'WORKASPACE' ) );
#12746 = CARTESIAN_POINT ( 'NONE',  ( -1.040834085586084257E-14, 25.49999999999996803, 52.49999999999998579 ) ) ;
#12747 = VERTEX_POINT ( 'NONE', #10878 ) ;
#12748 = CARTESIAN_POINT ( 'NONE',  ( -11.46040770435014977, -20.21908421996103655, 33.14257249208303335 ) ) ;
#12749 = EDGE_CURVE ( 'NONE', #12569, #1158, #9966, .T. ) ;
#12750 = EDGE_CURVE ( 'NONE', #15578, #10089, #13460, .T. ) ;
#12751 = CARTESIAN_POINT ( 'NONE',  ( -1.040834085586084257E-14, 25.49999999999998934, 52.50000000000000000 ) ) ;
#12752 = CARTESIAN_POINT ( 'NONE',  ( -15.16482700510262482, -20.99999999999997513, 37.73632249208304756 ) ) ;
#12753 = EDGE_LOOP ( 'NONE', ( #8723, #200, #8803, #15131, #205 ) ) ;
#12754 = CARTESIAN_POINT ( 'NONE',  ( -4.012830983233701687, 26.60336399182265055, 59.52836399182262994 ) ) ;
#12755 = ORIENTED_EDGE ( 'NONE', *, *, #8564, .T. ) ;
#12756 = CARTESIAN_POINT ( 'NONE',  ( 21.49999999999997513, 115.0000000000000000, -52.50000000000002132 ) ) ;
#12757 = EDGE_CURVE ( 'NONE', #13505, #2590, #9695, .T. ) ;
#12758 = LINE ( 'NONE', #19034, #8303 ) ;
#12759 = CARTESIAN_POINT ( 'NONE',  ( -24.00000000000000711, 53.00000000000000711, 1.500000000000001332 ) ) ;
#12760 = CARTESIAN_POINT ( 'NONE',  ( -40.00000000000000711, 110.0000000000000000, -38.50000000000000711 ) ) ;
#12761 =( NAMED_UNIT ( * ) SI_UNIT ( $, .STERADIAN. ) SOLID_ANGLE_UNIT ( ) );
#12762 = CARTESIAN_POINT ( 'NONE',  ( -37.50000000000002132, -6.000000000000000000, 24.99999999999998224 ) ) ;
#12763 = CARTESIAN_POINT ( 'NONE',  ( 1.300000000000000044, 0.7390083445627224634, 1.279999999999999138 ) ) ;
#12764 = EDGE_CURVE ( 'NONE', #9008, #14646, #17535, .T. ) ;
#12765 = ORIENTED_EDGE ( 'NONE', *, *, #6494, .T. ) ;
#12766 = CARTESIAN_POINT ( 'NONE',  ( -10.75228648362910100, -26.64274437364854009, 27.01367750791695954 ) ) ;
#12767 = CARTESIAN_POINT ( 'NONE',  ( -2.066987300000001415, 63.14382582708705627, 46.40000000109246514 ) ) ;
#12768 = CARTESIAN_POINT ( 'NONE',  ( -19.41254052147350961, -21.64274437364857562, 36.86132249208304046 ) ) ;
#12769 = AXIS2_PLACEMENT_3D ( 'NONE', #17910, #4481, #16427 ) ;
#12770 = FACE_OUTER_BOUND ( 'NONE', #1692, .T. ) ;
#12771 = CARTESIAN_POINT ( 'NONE',  ( -13.49542703274178379, -19.04416526290806289, 25.48242750791694888 ) ) ;
#12772 = DIRECTION ( 'NONE',  ( 1.047444401652940007E-14, 0.7071067811865495711, -0.7071067811865454633 ) ) ;
#12773 = CARTESIAN_POINT ( 'NONE',  ( -19.41254052147348830, -26.35725562635142083, 39.26367750791695954 ) ) ;
#12774 = CARTESIAN_POINT ( 'NONE',  ( 1.753982408753060218, -46.96461745799954457, 3.000000000000000000 ) ) ;
#12775 = CARTESIAN_POINT ( 'NONE',  ( -13.49542703274174116, -28.95583473709188738, 19.14257249208303691 ) ) ;
#12776 = PRODUCT_DEFINITION ( 'UNKNOWN', '', #11106, #13147 ) ;
#12777 = CARTESIAN_POINT ( 'NONE',  ( -1.767766952966369765, 62.23223304703363112, 49.29999999999999716 ) ) ;
#12778 = DIRECTION ( 'NONE',  ( 1.000000000000000000, 0.000000000000000000, 0.000000000000000000 ) ) ;
#12779 = CARTESIAN_POINT ( 'NONE',  ( 12.99999999999999822, 0.000000000000000000, 2.055000000000000160 ) ) ;
#12780 = CARTESIAN_POINT ( 'NONE',  ( -2.500000000000001776, 64.00000000000000000, 48.39999999999999858 ) ) ;
#12781 = LINE ( 'NONE', #18779, #193 ) ;
#12782 = AXIS2_PLACEMENT_3D ( 'NONE', #14254, #919, #6902 ) ;
#12783 = EDGE_LOOP ( 'NONE', ( #11516, #15110, #6661, #15221, #9491, #4649 ) ) ;
#12784 = SURFACE_STYLE_USAGE ( .BOTH. , #6817 ) ;
#12785 = CARTESIAN_POINT ( 'NONE',  ( 0.8561741729129460632, 66.06698730000000808, 45.30000000109246372 ) ) ;
#12786 = CARTESIAN_POINT ( 'NONE',  ( -14.83517299489739649, -18.99999999999997868, -0.9863224920830417908 ) ) ;
#12787 = CARTESIAN_POINT ( 'NONE',  ( -41.00000000000000711, 110.0000000000000000, 27.50000000000000000 ) ) ;
#12788 = CARTESIAN_POINT ( 'NONE',  ( -20.00369391078757886, -29.24501739517668142, 30.51757249208304401 ) ) ;
#12789 = AXIS2_PLACEMENT_3D ( 'NONE', #13106, #14492, #8420 ) ;
#12790 = CARTESIAN_POINT ( 'NONE',  ( -2.066987300000001415, 63.14382582708705627, 48.20000000109247651 ) ) ;
#12791 = VERTEX_POINT ( 'NONE', #4108 ) ;
#12792 = VECTOR ( 'NONE', #15499, 1000.000000000000114 ) ;
#12793 = PLANE ( 'NONE',  #14052 ) ;
#12794 = DIRECTION ( 'NONE',  ( -1.000000000000000000, 0.000000000000000000, -7.304098846218135653E-17 ) ) ;
#12795 = B_SPLINE_CURVE_WITH_KNOTS ( 'NONE', 3,
 ( #13552, #19252, #2672, #11884 ),
 .UNSPECIFIED., .F., .F.,
 ( 4, 4 ),
 ( 0.000000000000000000, 1.000000000000000000 ),
 .UNSPECIFIED. ) ;
#12796 = CARTESIAN_POINT ( 'NONE',  ( 2.066987300000001415, 64.00000000000000000, 46.75000000109247367 ) ) ;
#12797 = CARTESIAN_POINT ( 'NONE',  ( -1.040834085586084257E-14, 19.13603896932104220, 54.62132034355960286 ) ) ;
#12798 = DIRECTION ( 'NONE',  ( 0.000000000000000000, -0.7071067811865493491, 0.7071067811865456854 ) ) ;
#12799 = CARTESIAN_POINT ( 'NONE',  ( -41.00000000000000711, 110.0000000000000000, -18.00000000000000000 ) ) ;
#12800 = CARTESIAN_POINT ( 'NONE',  ( -7.999999999999986677, 60.00000000000000711, 66.99999999999997158 ) ) ;
#12801 = VERTEX_POINT ( 'NONE', #5478 ) ;
#12802 = ORIENTED_EDGE ( 'NONE', *, *, #9476, .T. ) ;
#12803 = CARTESIAN_POINT ( 'NONE',  ( -13.28918265808478694, -16.95583473709189093, 6.455072492083038682 ) ) ;
#12804 = AXIS2_PLACEMENT_3D ( 'NONE', #427, #8078, #5137 ) ;
#12805 = ORIENTED_EDGE ( 'NONE', *, *, #15127, .T. ) ;
#12806 = AXIS2_PLACEMENT_3D ( 'NONE', #14190, #6737, #17232 ) ;
#12808 = ORIENTED_EDGE ( 'NONE', *, *, #15721, .T. ) ;
#12807 = ORIENTED_EDGE ( 'NONE', *, *, #641, .F. ) ;
#12809 = CARTESIAN_POINT ( 'NONE',  ( -15.63902057219073605, -27.04416526290807710, 30.08007249208304401 ) ) ;
#12810 = ADVANCED_FACE ( 'NONE', ( #5206 ), #15688, .T. ) ;
#12811 = EDGE_CURVE ( 'NONE', #17473, #10091, #17435, .T. ) ;
#12812 = CARTESIAN_POINT ( 'NONE',  ( -12.95952864787955150, -17.04416526290805933, 30.73242750791696309 ) ) ;
#12813 = AXIS2_PLACEMENT_3D ( 'NONE', #14387, #16056, #963 ) ;
#12814 = CARTESIAN_POINT ( 'NONE',  ( -50.00000000000001421, 118.0000000000000142, 59.99999999999997868 ) ) ;
#12815 = CARTESIAN_POINT ( 'NONE',  ( 1.767766952966369987, 65.76776695296638309, 48.20000000218494307 ) ) ;
#12816 = ORIENTED_EDGE ( 'NONE', *, *, #2414, .T. ) ;
#12817 = ADVANCED_FACE ( 'NONE', ( #870 ), #4005, .T. ) ;
#12818 = DIRECTION ( 'NONE',  ( 0.000000000000000000, -0.5000000000000011102, -0.8660254037844379305 ) ) ;
#12819 = ORIENTED_EDGE ( 'NONE', *, *, #10329, .F. ) ;
#12820 = PLANE ( 'NONE',  #5034 ) ;
#12821 = ORIENTED_EDGE ( 'NONE', *, *, #9245, .T. ) ;
#12822 = CARTESIAN_POINT ( 'NONE',  ( -0.9169188819109246325, 62.14259808286531950, 45.00000000000001421 ) ) ;
#12823 = DIRECTION ( 'NONE',  ( 9.251858538542970348E-17, 0.000000000000000000, -1.000000000000000000 ) ) ;
#12824 = LINE ( 'NONE', #17073, #10943 ) ;
#12825 = EDGE_CURVE ( 'NONE', #14815, #2308, #17528, .T. ) ;
#12826 = VECTOR ( 'NONE', #16278, 1000.000000000000000 ) ;
#12827 = CARTESIAN_POINT ( 'NONE',  ( 1.461580736456473684, 65.46158073645646880, 46.05000000109246372 ) ) ;
#12828 = CONTEXT_DEPENDENT_SHAPE_REPRESENTATION ( #697, #13166 ) ;
#12829 = CARTESIAN_POINT ( 'NONE',  ( 12.55500000000001748, 0.000000000000000000, 0.000000000000000000 ) ) ;
#12830 = DIRECTION ( 'NONE',  ( -1.000000000000000000, -0.000000000000000000, -0.000000000000000000 ) ) ;
#12831 = PRESENTATION_LAYER_ASSIGNMENT (  '', '', ( #7849 ) ) ;
#12832 = LINE ( 'NONE', #15599, #14893 ) ;
#12833 = ORIENTED_EDGE ( 'NONE', *, *, #526, .T. ) ;
#12834 = EDGE_LOOP ( 'NONE', ( #9624, #9986, #13725, #12833 ) ) ;
#12835 = CARTESIAN_POINT ( 'NONE',  ( -20.24501739517664234, -29.00369391078761439, 2.294927507916956433 ) ) ;
#12836 = CARTESIAN_POINT ( 'NONE',  ( -24.00000000000000000, 53.00000000000000711, -32.00000000000000000 ) ) ;
#12837 = ORIENTED_EDGE ( 'NONE', *, *, #13937, .F. ) ;
#12838 = CARTESIAN_POINT ( 'NONE',  ( -10.75228648362912232, -21.35725562635138530, 33.36132249208304046 ) ) ;
#12839 = CIRCLE ( 'NONE', #1265, 2.500000000000000444 ) ;
#12840 = CARTESIAN_POINT ( 'NONE',  ( -5.800448837981398320, 29.71286850494553278, 56.77177811653244532 ) ) ;
#12841 = VERTEX_POINT ( 'NONE', #5393 ) ;
#12842 = CARTESIAN_POINT ( 'NONE',  ( -12.04416526290808420, -23.03132541760398766, 33.58007249208304756 ) ) ;
#12843 =( LENGTH_UNIT ( ) NAMED_UNIT ( * ) SI_UNIT ( .MILLI., .METRE. ) );
#12844 = ORIENTED_EDGE ( 'NONE', *, *, #3873, .T. ) ;
#12845 = DIRECTION ( 'NONE',  ( 1.000000000000000000, -0.000000000000000000, -0.000000000000000000 ) ) ;
#12846 = PRODUCT ( 'Removable Bottom Crumb Tray', 'Removable Bottom Crumb Tray', '', ( #3052 ) ) ;
#12847 = VERTEX_POINT ( 'NONE', #6764 ) ;
#12848 = PLANE ( 'NONE',  #2804 ) ;
#12849 = DIRECTION ( 'NONE',  ( -0.000000000000000000, -0.7071067811865493491, 0.7071067811865456854 ) ) ;
#12850 = CARTESIAN_POINT ( 'NONE',  ( 1.000000000000001998, -32.00000000000000000, 4.500000000000000888 ) ) ;
#12851 = AXIS2_PLACEMENT_3D ( 'NONE', #11986, #10713, #4555 ) ;
#12852 = VECTOR ( 'NONE', #16959, 1000.000000000000000 ) ;
#12853 = EDGE_CURVE ( 'NONE', #5207, #5173, #5574, .T. ) ;
#12854 = CARTESIAN_POINT ( 'NONE',  ( -9.955834737091912245, -22.82508104294696594, 31.60742750791695954 ) ) ;
#12855 = ADVANCED_FACE ( 'NONE', ( #11532 ), #12820, .F. ) ;
#12856 = CARTESIAN_POINT ( 'NONE',  ( -1.040834085586084257E-14, 34.69238815542512100, 47.55025253169419841 ) ) ;
#12857 = EDGE_CURVE ( 'NONE', #19005, #2170, #14212, .T. ) ;
#12858 = CYLINDRICAL_SURFACE ( 'NONE', #9885, 2.500000000000002220 ) ;
#12859 = LINE ( 'NONE', #6982, #16808 ) ;
#12860 = ORIENTED_EDGE ( 'NONE', *, *, #2677, .T. ) ;
#12861 = AXIS2_PLACEMENT_3D ( 'NONE', #6458, #6555, #9482 ) ;
#12862 = ORIENTED_EDGE ( 'NONE', *, *, #18539, .F. ) ;
#12863 = VECTOR ( 'NONE', #18555, 1000.000000000000000 ) ;
#12864 = CARTESIAN_POINT ( 'NONE',  ( -16.50457296725820555, -28.95583473709189448, 28.10742750791695954 ) ) ;
#12865 = CARTESIAN_POINT ( 'NONE',  ( 2.066987300000002303, 63.14382582708705627, 48.30000000109247082 ) ) ;
#12866 = CARTESIAN_POINT ( 'NONE',  ( -14.83517299489735741, -28.99999999999998224, 29.86132249208304401 ) ) ;
#12867 =( BOUNDED_CURVE ( )  B_SPLINE_CURVE ( 2, ( #720, #12669, #3468, #9444, #12474, #2284, #6700, #18670, #8269 ),
 .UNSPECIFIED., .F., .F. ) 
 B_SPLINE_CURVE_WITH_KNOTS ( ( 3, 2, 2, 2, 3 ),
 ( 0.5714285714285711748, 0.5892857142857141906, 0.6071428571428569843, 0.6250000000000000000, 0.6428571428571429047 ),
 .UNSPECIFIED. ) 
 CURVE ( )  GEOMETRIC_REPRESENTATION_ITEM ( )  RATIONAL_B_SPLINE_CURVE ( ( 1.000000000000000888, 0.9238795325112857393, 1.000000000000000000, 0.9238795325112867385, 1.000000000000000000, 0.9238795325112867385, 1.000000000000000000, 0.9238795325112867385, 1.000000000000000000 ) ) 
 REPRESENTATION_ITEM ( '' )  );
#12868 = MECHANICAL_DESIGN_GEOMETRIC_PRESENTATION_REPRESENTATION (  '', ( #3160 ), #9443 ) ;
#12869 = CARTESIAN_POINT ( 'NONE',  ( -25.00000000000000000, 110.0000000000000000, -11.50000000000000355 ) ) ;
#12870 = CARTESIAN_POINT ( 'NONE',  ( 0.1499999999999973577, 3.367778697655221012E-16, -2.750000000000000000 ) ) ;
#12871 = CARTESIAN_POINT ( 'NONE',  ( -20.04416526290808065, -25.17491895705300209, 34.23242750791695954 ) ) ;
#12872 = DIRECTION ( 'NONE',  ( -0.000000000000000000, -1.000000000000000000, -0.000000000000000000 ) ) ;
#12873 = CARTESIAN_POINT ( 'NONE',  ( -14.83517299489739649, -18.99999999999997868, 30.51367750791695954 ) ) ;
#12874 = CARTESIAN_POINT ( 'NONE',  ( -4.189607678530337331, 26.72836399182265055, 59.40336399182262284 ) ) ;
#12875 = CARTESIAN_POINT ( 'NONE',  ( 4.012830983233651061, 32.52836399182262994, 53.60336399182268252 ) ) ;
#12876 = EDGE_CURVE ( 'NONE', #3207, #4412, #6848, .T. ) ;
#12877 = EDGE_CURVE ( 'NONE', #12352, #16642, #17341, .T. ) ;
#12878 = CARTESIAN_POINT ( 'NONE',  ( -1.461580736456473906, 65.46158073645646880, 45.65000000109247225 ) ) ;
#12879 = AXIS2_PLACEMENT_3D ( 'NONE', #11764, #18940, #2656 ) ;
#12880 = LINE ( 'NONE', #2488, #11790 ) ;
#12881 = CARTESIAN_POINT ( 'NONE',  ( -2.500000000000001776, 64.00000000000000000, 49.19999999999999574 ) ) ;
#12882 = LINE ( 'NONE', #9929, #11448 ) ;
#12883 = CIRCLE ( 'NONE', #5089, 2.649999999999985700 ) ;
#12884 = ORIENTED_EDGE ( 'NONE', *, *, #665, .F. ) ;
#12885 =( NAMED_UNIT ( * ) PLANE_ANGLE_UNIT ( ) SI_UNIT ( $, .RADIAN. ) );
#12886 = DIRECTION ( 'NONE',  ( 1.000000000000000000, 0.000000000000000000, 0.000000000000000000 ) ) ;
#12887 = CARTESIAN_POINT ( 'NONE',  ( -10.75228648362910100, -26.64274437364854009, 6.013677507916958653 ) ) ;
#12888 = CARTESIAN_POINT ( 'NONE',  ( 2.500000000000001776, 64.00000000000000000, 49.99999999999999289 ) ) ;
#12889 = CARTESIAN_POINT ( 'NONE',  ( -12.95952864787948755, -30.95583473709188382, 29.64257249208304401 ) ) ;
#12890 = CARTESIAN_POINT ( 'NONE',  ( -2.066987300000001415, 64.00000000000000000, 48.95000000109246940 ) ) ;
#12891 = ORIENTED_EDGE ( 'NONE', *, *, #9348, .F. ) ;
#12892 = LINE ( 'NONE', #11137, #16559 ) ;
#12893 = DIRECTION ( 'NONE',  ( 0.000000000000000000, 0.7071067811865456854, 0.7071067811865494601 ) ) ;
#12894 = EDGE_CURVE ( 'NONE', #12535, #12747, #5291, .T. ) ;
#12895 = CARTESIAN_POINT ( 'NONE',  ( -1.461580736456473906, 65.46158073645646880, 47.05000000109247082 ) ) ;
#12896 = DIRECTION ( 'NONE',  ( -1.000000000000000000, -0.000000000000000000, -0.000000000000000000 ) ) ;
#12897 = CARTESIAN_POINT ( 'NONE',  ( -1.035533905932738641, 66.50000000000000000, 49.15000000218494591 ) ) ;
#12898 = VECTOR ( 'NONE', #4503, 1000.000000000000000 ) ;
#12899 = DIRECTION ( 'NONE',  ( 0.000000000000000000, 1.000000000000000000, -1.471414886128461669E-15 ) ) ;
#12900 = CARTESIAN_POINT ( 'NONE',  ( -37.50000000000002132, 0.000000000000000000, 24.99999999999998224 ) ) ;
#12901 = ORIENTED_EDGE ( 'NONE', *, *, #16599, .F. ) ;
#12902 = ORIENTED_EDGE ( 'NONE', *, *, #9858, .F. ) ;
#12903 = CARTESIAN_POINT ( 'NONE',  ( -8.855408670957602979, -27.35725562635137820, 7.986322492083039570 ) ) ;
#12904 =( LENGTH_UNIT ( ) NAMED_UNIT ( * ) SI_UNIT ( .MILLI., .METRE. ) );
#12905 = ORIENTED_EDGE ( 'NONE', *, *, #13689, .F. ) ;
#12907 = ORIENTED_EDGE ( 'NONE', *, *, #11452, .F. ) ;
#12906 = ORIENTED_EDGE ( 'NONE', *, *, #15975, .T. ) ;
#12908 = CARTESIAN_POINT ( 'NONE',  ( -12.48433729119798130, -25.64274437364855075, 6.013677507916959541 ) ) ;
#12909 = CARTESIAN_POINT ( 'NONE',  ( -11.35725562635144925, -18.02023567606020293, 30.95117750791695954 ) ) ;
#12910 = CARTESIAN_POINT ( 'NONE',  ( -41.00000000000000711, 53.00000000000000711, 14.50000000000000000 ) ) ;
#12911 = CARTESIAN_POINT ( 'NONE',  ( 2.500000000000001776, 65.03553390593273775, 48.95000000218495018 ) ) ;
#12912 = CARTESIAN_POINT ( 'NONE',  ( -3.155775640247338920, -38.39960408384397539, 3.000000000000000000 ) ) ;
#12913 = ORIENTED_EDGE ( 'NONE', *, *, #8995, .T. ) ;
#12914 = FACE_OUTER_BOUND ( 'NONE', #18153, .T. ) ;
#12915 = ORIENTED_EDGE ( 'NONE', *, *, #8785, .T. ) ;
#12916 = EDGE_CURVE ( 'NONE', #885, #17434, #8514, .T. ) ;
#12917 = DIRECTION ( 'NONE',  ( -0.000000000000000000, -1.000000000000000000, -0.000000000000000000 ) ) ;
#12918 = ORIENTED_EDGE ( 'NONE', *, *, #4485, .T. ) ;
#12919 = FACE_OUTER_BOUND ( 'NONE', #14378, .T. ) ;
#12920 = EDGE_CURVE ( 'NONE', #2343, #11653, #12640, .T. ) ;
#12921 = CARTESIAN_POINT ( 'NONE',  ( -24.00000000000000000, 53.00000000000000711, 30.00000000000000000 ) ) ;
#12922 = CARTESIAN_POINT ( 'NONE',  ( -3.400000000000017675, 29.47747564417433352, 56.65425233947095052 ) ) ;
#12923 = CARTESIAN_POINT ( 'NONE',  ( 0.8561741729129472844, 61.93301270000000613, 49.20000000109247651 ) ) ;
#12924 = DIRECTION ( 'NONE',  ( 0.000000000000000000, 0.000000000000000000, 1.000000000000000000 ) ) ;
#12925 = FACE_OUTER_BOUND ( 'NONE', #10973, .T. ) ;
#12926 = CARTESIAN_POINT ( 'NONE',  ( -12.50000000000000000, -35.50000000000000000, 5.500000000000000000 ) ) ;
#12927 = VERTEX_POINT ( 'NONE', #7039 ) ;
#12928 = EDGE_LOOP ( 'NONE', ( #5318, #12379, #4817, #5016 ) ) ;
#12929 = CARTESIAN_POINT ( 'NONE',  ( -20.97976432393977575, -20.35725562635143504, 8.638677507916955989 ) ) ;
#12930 = CARTESIAN_POINT ( 'NONE',  ( -40.00000000000000711, 110.0000000000000000, -30.99999999999999645 ) ) ;
#12931 = ORIENTED_EDGE ( 'NONE', *, *, #1518, .F. ) ;
#12932 = CARTESIAN_POINT ( 'NONE',  ( -19.99999999999999645, -24.16482700510261949, 41.67382249208304046 ) ) ;
#12933 = CARTESIAN_POINT ( 'NONE',  ( -1.530808498934192803E-16, 66.50000000000000000, 45.79999999999999005 ) ) ;
#12934 = ORIENTED_EDGE ( 'NONE', *, *, #15152, .T. ) ;
#12935 = EDGE_CURVE ( 'NONE', #16140, #14750, #19009, .T. ) ;
#12936 = CARTESIAN_POINT ( 'NONE',  ( -13.64274437364857739, -21.31951028609534760, 38.17382249208304046 ) ) ;
#12937 = ORIENTED_EDGE ( 'NONE', *, *, #17165, .F. ) ;
#12938 = CARTESIAN_POINT ( 'NONE',  ( 1.035533905932738197, 66.50000000000000000, 46.65000000218494591 ) ) ;
#12939 = ORIENTED_EDGE ( 'NONE', *, *, #12508, .T. ) ;
#12940 = PLANE ( 'NONE',  #11247 ) ;
#12941 = FACE_OUTER_BOUND ( 'NONE', #14928, .T. ) ;
#12942 = DIRECTION ( 'NONE',  ( -1.000000000000000000, -0.000000000000000000, -0.000000000000000000 ) ) ;
#12943 = EDGE_CURVE ( 'NONE', #17726, #9708, #8152, .T. ) ;
#12944 = CARTESIAN_POINT ( 'NONE',  ( -13.82508104294698192, -29.04416526290806644, 27.66992750791695244 ) ) ;
#12945 = VECTOR ( 'NONE', #9156, 1000.000000000000000 ) ;
#12946 = CARTESIAN_POINT ( 'NONE',  ( -1.485306817036799787, -35.74454190283287147, 7.499999999999995559 ) ) ;
#12947 = LINE ( 'NONE', #5327, #11614 ) ;
#12948 = DIRECTION ( 'NONE',  ( 0.7071067811865535679, 0.4999999999999973355, -0.4999999999999940048 ) ) ;
#12949 = PLANE ( 'NONE',  #1128 ) ;
#12950 = ORIENTED_EDGE ( 'NONE', *, *, #12281, .T. ) ;
#12951 = CARTESIAN_POINT ( 'NONE',  ( -18.35725562635138886, -30.14459132904237393, 35.54882249208304046 ) ) ;
#12952 = CARTESIAN_POINT ( 'NONE',  ( -14.83517299489739649, -18.99999999999997868, 30.51367750791695954 ) ) ;
#12953 = CARTESIAN_POINT ( 'NONE',  ( -1.265664690411616068E-16, 66.06698730000000808, 47.75000000109246656 ) ) ;
#12954 = CARTESIAN_POINT ( 'NONE',  ( -16.50457296725825174, -19.04416526290807354, 32.26757249208304046 ) ) ;
#12955 = MECHANICAL_DESIGN_GEOMETRIC_PRESENTATION_REPRESENTATION (  '', ( #13275 ), #17989 ) ;
#12956 = CARTESIAN_POINT ( 'NONE',  ( 8.000000000000003553, 0.000000000000000000, 0.000000000000000000 ) ) ;
#12957 = EDGE_LOOP ( 'NONE', ( #16949, #459 ) ) ;
#12958 = EDGE_CURVE ( 'NONE', #11043, #2345, #14087, .T. ) ;
#12959 = AXIS2_PLACEMENT_3D ( 'NONE', #8001, #9550, #6807 ) ;
#12960 = FACE_OUTER_BOUND ( 'NONE', #290, .T. ) ;
#12961 = CARTESIAN_POINT ( 'NONE',  ( -19.41254052147348830, -26.35725562635142083, 23.51367750791695954 ) ) ;
#12962 = ADVANCED_FACE ( 'NONE', ( #1635 ), #8606, .F. ) ;
#12963 = CARTESIAN_POINT ( 'NONE',  ( -41.00000000000000711, 113.0000000000000000, 30.00000000000000000 ) ) ;
#12964 = CARTESIAN_POINT ( 'NONE',  ( -2.315774708385926139, 31.32836399182264842, 54.80336399182263563 ) ) ;
#12965 = CARTESIAN_POINT ( 'NONE',  ( -25.00000000000000711, 110.0000000000000000, -38.50000000000000711 ) ) ;
#12966 = LINE ( 'NONE', #17389, #649 ) ;
#12967 = CARTESIAN_POINT ( 'NONE',  ( -2.066987300000001415, 64.00000000000000000, 44.95000000109246940 ) ) ;
#12968 = CARTESIAN_POINT ( 'NONE',  ( -2.066987300000000971, 63.14382582708704916, 49.00000000109246656 ) ) ;
#12969 = CARTESIAN_POINT ( 'NONE',  ( -1.767766952966369765, 62.23223304703363112, 48.60000000218494165 ) ) ;
#12970 = CARTESIAN_POINT ( 'NONE',  ( 1.767766952966369987, 65.76776695296638309, 48.89999999999999858 ) ) ;
#12971 = LINE ( 'NONE', #5735, #7080 ) ;
#12972 = VECTOR ( 'NONE', #1530, 1000.000000000000000 ) ;
#12973 = VERTEX_POINT ( 'NONE', #7606 ) ;
#12974 =( BOUNDED_CURVE ( )  B_SPLINE_CURVE ( 2, ( #6460, #382, #3605, #12330, #4993, #7737, #4702, #12524, #6264, #669, #4897, #10658, #473, #12428, #10857, #18126, #16852, #13699, #10950, #16660, #3413, #13996, #10755, #3225, #15471, #9575, #12232, #18231, #8031, #4806, #18524, #278, #9384, #566, #6557, #8392, #14367, #14564, #15848, #17411, #942, #15939, #12617, #5552, #17135, #8491, #12984, #11328, #11507, #2410, #12895, #17501, #845, #18984, #6924, #17231, #12796, #4078, #8583, #12705, #9941, #18894, #18706, #7015, #1136, #18612, #11139, #5456, #11417, #3983, #5178, #2506, #14468, #1040, #6826, #6736, #10045, #753, #16041, #2601, #15759, #3698, #9671, #15662, #2232, #18793, #8224, #14189, #3800, #5369, #5269, #11225, #9766 ),
 .UNSPECIFIED., .F., .F. ) 
 B_SPLINE_CURVE_WITH_KNOTS ( ( 3, 2, 2, 2, 2, 2, 2, 2, 2, 2, 2, 2, 2, 2, 2, 2, 2, 2, 2, 2, 2, 2, 2, 2, 2, 2, 2, 2, 2, 2, 2, 2, 2, 2, 2, 2, 2, 2, 2, 2, 2, 2, 2, 2, 2, 2, 3 ),
 ( 0.000000000000000000, 0.01785714285714285615, 0.03571428571428571230, 0.05357142857142856845, 0.07142857142857142461, 0.08928571428571428770, 0.1071428571428571369, 0.1250000000000000000, 0.1428571428571428492, 0.1607142857142857262, 0.1785714285714285754, 0.1964285714285714246, 0.2142857142857142738, 0.2321428571428571508, 0.2500000000000000000, 0.2678571428571428492, 0.2857142857142856984, 0.3035714285714285476, 0.3214285714285714524, 0.3392857142857143016, 0.3571428571428571508, 0.3750000000000000000, 0.3928571428571428492, 0.4107142857142856984, 0.4285714285714285476, 0.4464285714285714524, 0.4642857142857143016, 0.4821428571428571508, 0.5000000000000000000, 0.5178571428571429047, 0.5357142857142856984, 0.5535714285714286031, 0.5714285714285713969, 0.5892857142857143016, 0.6071428571428570953, 0.6250000000000000000, 0.6428571428571429047, 0.6607142857142856984, 0.6785714285714286031, 0.6964285714285713969, 0.7142857142857143016, 0.7321428571428570953, 0.7500000000000000000, 0.7678571428571429047, 0.7857142857142856984, 0.8035714285714286031, 0.8125000001876604427 ),
 .UNSPECIFIED. ) 
 CURVE ( )  GEOMETRIC_REPRESENTATION_ITEM ( )  RATIONAL_B_SPLINE_CURVE ( ( 1.000000000000000000, 0.9238795325112867385, 1.000000000000000000, 0.9238795325112867385, 1.000000000000000000, 0.9238795325112867385, 1.000000000000000000, 0.9238795325112867385, 1.000000000000000000, 0.9238795325112867385, 1.000000000000000000, 0.9238795325112867385, 1.000000000000000000, 0.9238795325112867385, 1.000000000000000000, 0.9238795325112867385, 1.000000000000000000, 0.9238795325112867385, 1.000000000000000000, 0.9238795325112867385, 1.000000000000000000, 0.9238795325112867385, 1.000000000000000000, 0.9238795325112867385, 1.000000000000000000, 0.9238795325112867385, 1.000000000000000000, 0.9238795325112867385, 1.000000000000000000, 0.9238795325112867385, 1.000000000000000000, 0.9238795325112867385, 1.000000000000000000, 0.9238795325112867385, 1.000000000000000000, 0.9238795325112867385, 1.000000000000000000, 0.9238795325112867385, 1.000000000000000000, 0.9238795325112867385, 1.000000000000000000, 0.9238795325112867385, 1.000000000000000000, 0.9238795325112867385, 1.000000000000000000, 0.9238795325112867385, 1.000000000000000000, 0.9238795325112867385, 1.000000000000000000, 0.9238795325112867385, 1.000000000000000000, 0.9238795325112867385, 1.000000000000000000, 0.9238795325112867385, 1.000000000000000000, 0.9238795325112867385, 1.000000000000000000, 0.9238795325112867385, 1.000000000000000000, 0.9238795325112867385, 1.000000000000000000, 0.9238795325112867385, 1.000000000000000000, 0.9238795325112867385, 1.000000000000000000, 0.9238795325112867385, 1.000000000000000000, 0.9238795325112867385, 1.000000000000000000, 0.9238795325112867385, 1.000000000000000000, 0.9238795325112867385, 1.000000000000000000, 0.9238795325112867385, 1.000000000000000000, 0.9238795325112867385, 1.000000000000000000, 0.9238795325112867385, 1.000000000000000000, 0.9238795325112867385, 1.000000000000000000, 0.9238795325112867385, 1.000000000000000000, 0.9238795325112867385, 1.000000000000000000, 0.9238795325112867385, 1.000000000000000000, 0.9238795325112867385, 1.000000000000000000, 0.9238795325112867385, 1.000000000000000000, 0.9619397654556944843, 0.9619397662556434803 ) ) 
 REPRESENTATION_ITEM ( '' )  );
#12975 = CARTESIAN_POINT ( 'NONE',  ( 3.796994071234847710E-16, 61.93301269999999903, 45.75000000109247367 ) ) ;
#12976 = CARTESIAN_POINT ( 'NONE',  ( -19.24771351637089367, -21.35725562635142438, 3.388677507916958653 ) ) ;
#12977 = DIRECTION ( 'NONE',  ( 0.000000000000000000, 1.000000000000000000, 0.000000000000000000 ) ) ;
#12978 = CARTESIAN_POINT ( 'NONE',  ( -21.95583473709189803, -26.04047135212049469, 36.20507249208304046 ) ) ;
#12979 = EDGE_CURVE ( 'NONE', #9696, #15107, #13375, .T. ) ;
#12980 = CARTESIAN_POINT ( 'NONE',  ( -2.066987300000001859, 64.85617417291294373, 44.70000000109248361 ) ) ;
#12981 = CARTESIAN_POINT ( 'NONE',  ( -1.040834085586084257E-14, 29.74264068711925901, 56.74264068711929809 ) ) ;
#12982 = CARTESIAN_POINT ( 'NONE',  ( -15.00000000000000000, 0.000000000000000000, 33.99999999999999289 ) ) ;
#12983 = TOROIDAL_SURFACE ( 'NONE', #13614, 1.600000000000000311, 0.1000000000000000056 ) ;
#12984 = CARTESIAN_POINT ( 'NONE',  ( -1.461580736456473462, 62.53841926354353120, 47.25000000109247367 ) ) ;
#12985 = CARTESIAN_POINT ( 'NONE',  ( -5.800000000000005151, 29.74264068711930520, 56.74264068711926257 ) ) ;
#12986 = CARTESIAN_POINT ( 'NONE',  ( 1.035533905932738197, 66.50000000000000000, 49.05000000218495160 ) ) ;
#12987 = CYLINDRICAL_SURFACE ( 'NONE', #19123, 2.499999999999998668 ) ;
#12988 = LINE ( 'NONE', #2605, #2073 ) ;
#12989 = VERTEX_POINT ( 'NONE', #10625 ) ;
#12990 = EDGE_LOOP ( 'NONE', ( #2717, #7356, #4413, #18545, #18047, #4909, #3262, #743 ) ) ;
#12991 = CARTESIAN_POINT ( 'NONE',  ( -8.044165262908093084, -21.95952864787946979, 2.080072492083039126 ) ) ;
#12992 = VECTOR ( 'NONE', #12040, 1000.000000000000000 ) ;
#12993 = ORIENTED_EDGE ( 'NONE', *, *, #17683, .F. ) ;
#12994 = VECTOR ( 'NONE', #14496, 1000.000000000000000 ) ;
#12996 = ORIENTED_EDGE ( 'NONE', *, *, #15511, .F. ) ;
#12995 = ORIENTED_EDGE ( 'NONE', *, *, #3795, .T. ) ;
#12997 = PRODUCT ( 'Heating Element & carriage', 'Heating Element & carriage', '', ( #15 ) ) ;
#12998 = ADVANCED_FACE ( 'NONE', ( #4477 ), #7500, .F. ) ;
#12999 = CARTESIAN_POINT ( 'NONE',  ( -13.35725562635141195, -26.51566270880198672, 39.92382249208304756 ) ) ;
#13000 = CARTESIAN_POINT ( 'NONE',  ( -20.97976432393977575, -20.35725562635143504, 29.63867750791695954 ) ) ;
#13001 = DIRECTION ( 'NONE',  ( -0.000000000000000000, -1.000000000000000000, -0.000000000000000000 ) ) ;
#13002 = CARTESIAN_POINT ( 'NONE',  ( 2.500000000000001776, 65.03553390593273775, 48.15000000218494591 ) ) ;
#13003 = CARTESIAN_POINT ( 'NONE',  ( 1.844224359752661968, -41.39960408384398249, 3.000000000000000000 ) ) ;
#13004 = ORIENTED_EDGE ( 'NONE', *, *, #12310, .T. ) ;
#13005 = CARTESIAN_POINT ( 'NONE',  ( -4.189131392896543460, 32.57932772728320003, 53.90500129688591358 ) ) ;
#13006 = VERTEX_POINT ( 'NONE', #16724 ) ;
#13007 = DIRECTION ( 'NONE',  ( -0.000000000000000000, -0.000000000000000000, -1.000000000000000000 ) ) ;
#13008 = ORIENTED_EDGE ( 'NONE', *, *, #17300, .T. ) ;
#13009 = DIRECTION ( 'NONE',  ( 0.7071067811865390240, -0.5000000000000073275, 0.5000000000000048850 ) ) ;
#13010 = EDGE_CURVE ( 'NONE', #8618, #2690, #6338, .T. ) ;
#13011 = PLANE ( 'NONE',  #2778 ) ;
#13012 = DIRECTION ( 'NONE',  ( 0.000000000000000000, 0.000000000000000000, 1.000000000000000000 ) ) ;
#13013 = CIRCLE ( 'NONE', #14926, 1.599999999999997202 ) ;
#13014 = CARTESIAN_POINT ( 'NONE',  ( -1.265664690411616068E-16, 66.06698730000000808, 44.55000000109247082 ) ) ;
#13015 = CIRCLE ( 'NONE', #10185, 2.999999999999999112 ) ;
#13016 = DIRECTION ( 'NONE',  ( 5.782411586589357392E-17, -0.000000000000000000, 1.000000000000000000 ) ) ;
#13017 = DIRECTION ( 'NONE',  ( 1.000000000000000000, 0.000000000000000000, 0.000000000000000000 ) ) ;
#13018 = DIRECTION ( 'NONE',  ( 1.000000000000000000, 0.000000000000000000, 0.000000000000000000 ) ) ;
#13019 = ORIENTED_EDGE ( 'NONE', *, *, #13961, .F. ) ;
#13021 = VERTEX_POINT ( 'NONE', #14589 ) ;
#13020 = EDGE_LOOP ( 'NONE', ( #14499, #2822, #97, #816 ) ) ;
#13022 = CARTESIAN_POINT ( 'NONE',  ( -20.04416526290808065, -25.17491895705300209, 39.48242750791695244 ) ) ;
#13023 = DIRECTION ( 'NONE',  ( -1.000000000000000000, 0.000000000000000000, 0.000000000000000000 ) ) ;
#13024 = ORIENTED_EDGE ( 'NONE', *, *, #8836, .F. ) ;
#13025 = CARTESIAN_POINT ( 'NONE',  ( -17.99999999999999645, -24.16482700510260173, 10.17382249208304223 ) ) ;
#13026 = AXIS2_PLACEMENT_3D ( 'NONE', #7078, #16009, #5331 ) ;
#13027 = CIRCLE ( 'NONE', #7403, 2.500000000000001776 ) ;
#13028 = CARTESIAN_POINT ( 'NONE',  ( -1.035533905932738641, 66.50000000000000000, 45.04999999999999005 ) ) ;
#13029 = ORIENTED_EDGE ( 'NONE', *, *, #5881, .F. ) ;
#13030 = CARTESIAN_POINT ( 'NONE',  ( -16.64274437364856496, -26.51566270880199738, 2.076177507916959986 ) ) ;
#13031 = ORIENTED_EDGE ( 'NONE', *, *, #15261, .T. ) ;
#13032 = CARTESIAN_POINT ( 'NONE',  ( 2.499999999999999112, 65.03553390593273775, 46.55000000218494449 ) ) ;
#13033 = ORIENTED_EDGE ( 'NONE', *, *, #3850, .T. ) ;
#13034 = CARTESIAN_POINT ( 'NONE',  ( 1.300000000000000044, -1.478016689125442706, 1.843143693225357538E-15 ) ) ;
#13035 = DIRECTION ( 'NONE',  ( -1.000000000000000000, 0.000000000000000000, 0.000000000000000000 ) ) ;
#13036 = DIRECTION ( 'NONE',  ( -0.000000000000000000, -0.7071067811865456854, -0.7071067811865493491 ) ) ;
#13037 = CARTESIAN_POINT ( 'NONE',  ( -9.183694056713489507E-15, 18.42893218813449607, 59.57106781186546129 ) ) ;
#13038 =( GEOMETRIC_REPRESENTATION_CONTEXT ( 3 ) GLOBAL_UNCERTAINTY_ASSIGNED_CONTEXT ( ( #8274 ) ) GLOBAL_UNIT_ASSIGNED_CONTEXT ( ( #12904, #17144, #3993 ) ) REPRESENTATION_CONTEXT ( 'NONE', 'WORKASPACE' ) );
#13039 = CARTESIAN_POINT ( 'NONE',  ( -19.41254052147348830, -26.35725562635142083, 28.76367750791695954 ) ) ;
#13040 = FACE_BOUND ( 'NONE', #2632, .T. ) ;
#13041 = CARTESIAN_POINT ( 'NONE',  ( -16.17491895705301275, -18.95583473709189803, 4.044927507916959541 ) ) ;
#13042 = DIRECTION ( 'NONE',  ( 0.000000000000000000, 0.000000000000000000, -1.000000000000000000 ) ) ;
#13043 = VERTEX_POINT ( 'NONE', #19367 ) ;
#13044 = CARTESIAN_POINT ( 'NONE',  ( -17.35725562635140307, -28.41254052147349185, 9.298822492083040459 ) ) ;
#13045 = CARTESIAN_POINT ( 'NONE',  ( -8.044165262908075320, -26.04047135212042718, 0.5449275079169564329 ) ) ;
#13046 = CARTESIAN_POINT ( 'NONE',  ( -2.066987300000001415, 64.00000000000000000, 47.15000000109247225 ) ) ;
#13047 = ADVANCED_FACE ( 'NONE', ( #12303 ), #152, .F. ) ;
#13048 = ADVANCED_FACE ( 'NONE', ( #15153 ), #6138, .T. ) ;
#13049 = CARTESIAN_POINT ( 'NONE',  ( -15.16482700510262482, -20.99999999999997513, 11.48632249208304223 ) ) ;
#13050 = CARTESIAN_POINT ( 'NONE',  ( 3.000000000000002665, 0.000000000000000000, 0.000000000000000000 ) ) ;
#13051 = ORIENTED_EDGE ( 'NONE', *, *, #12135, .F. ) ;
#13052 = CARTESIAN_POINT ( 'NONE',  ( -2.500000000000001776, 64.00000000000000000, 46.10000000218494165 ) ) ;
#13053 = CARTESIAN_POINT ( 'NONE',  ( -19.99999999999999645, -23.83517299489738051, 34.45117750791696665 ) ) ;
#13054 = EDGE_CURVE ( 'NONE', #10947, #7234, #249, .T. ) ;
#13055 = CARTESIAN_POINT ( 'NONE',  ( -0.000000000000000000, -32.00000000000000711, 0.000000000000000000 ) ) ;
#13056 = CARTESIAN_POINT ( 'NONE',  ( 4.000000000000000888, 52.00000000000000711, 30.00000000000000000 ) ) ;
#13057 = CARTESIAN_POINT ( 'NONE',  ( 0.000000000000000000, 64.00000000000000000, 49.99999999999999289 ) ) ;
#13058 = CARTESIAN_POINT ( 'NONE',  ( -12.35725562635140307, -28.24771351637085459, 39.92382249208304046 ) ) ;
#13059 =( REPRESENTATION_RELATIONSHIP ('NONE','NONE', #7912, #3576 ) REPRESENTATION_RELATIONSHIP_WITH_TRANSFORMATION ( #10886 )SHAPE_REPRESENTATION_RELATIONSHIP( ) );
#13060 = CARTESIAN_POINT ( 'NONE',  ( 2.500000000000001776, 65.03553390593273775, 48.04999999999999716 ) ) ;
#13061 = CARTESIAN_POINT ( 'NONE',  ( -1.461580736456473462, 62.53841926354353120, 49.05000000109247082 ) ) ;
#13062 = EDGE_CURVE ( 'NONE', #15286, #19005, #10067, .T. ) ;
#13063 = CARTESIAN_POINT ( 'NONE',  ( -3.155775640247338920, -41.39960408384398249, 3.000000000000000000 ) ) ;
#13064 = CARTESIAN_POINT ( 'NONE',  ( 2.500000000000002220, 62.96446609406726935, 48.74999999999999289 ) ) ;
#13065 = LINE ( 'NONE', #19061, #18676 ) ;
#13066 = EDGE_LOOP ( 'NONE', ( #5100, #1145, #8255, #3134 ) ) ;
#13067 = EDGE_CURVE ( 'NONE', #1273, #3857, #18201, .T. ) ;
#13068 = CARTESIAN_POINT ( 'NONE',  ( -9.999999999999994671, -24.16482700510257686, 0.3261775079169582647 ) ) ;
#13069 = CARTESIAN_POINT ( 'NONE',  ( -20.04416526290808065, -25.17491895705300209, 2.732427507916957765 ) ) ;
#13070 = FACE_OUTER_BOUND ( 'NONE', #10475, .T. ) ;
#13071 = CARTESIAN_POINT ( 'NONE',  ( -18.35725562635138886, -30.14459132904237393, 30.29882249208304401 ) ) ;
#13072 = CARTESIAN_POINT ( 'NONE',  ( 3.796994071234847710E-16, 61.93301269999999903, 47.55000000109247082 ) ) ;
#13073 = EDGE_CURVE ( 'NONE', #89, #1447, #10728, .T. ) ;
#13074 = CARTESIAN_POINT ( 'NONE',  ( -17.07549068051210739, -21.68318583509881847, 35.10742750791696665 ) ) ;
#13075 = CARTESIAN_POINT ( 'NONE',  ( -12.64274437364855252, -28.41254052147347053, 1.201177507916958431 ) ) ;
#13076 = LINE ( 'NONE', #7014, #16645 ) ;
#13077 = CARTESIAN_POINT ( 'NONE',  ( -2.066987300000001415, 64.00000000000000000, 49.75000000109246656 ) ) ;
#13078 = CARTESIAN_POINT ( 'NONE',  ( -25.00000000000000000, 110.0000000000000000, -44.00000000000000000 ) ) ;
#13079 = AXIS2_PLACEMENT_3D ( 'NONE', #18003, #4578, #9074 ) ;
#13080 = CARTESIAN_POINT ( 'NONE',  ( -2.500000000000001776, 65.03553390593273775, 49.94999999999998863 ) ) ;
#13081 = CARTESIAN_POINT ( 'NONE',  ( 2.066987300000001415, 64.00000000000000000, 48.55000000109247082 ) ) ;
#13082 = FACE_OUTER_BOUND ( 'NONE', #96, .T. ) ;
#13083 = EDGE_CURVE ( 'NONE', #3007, #15605, #18298, .T. ) ;
#13084 = EDGE_CURVE ( 'NONE', #14775, #6698, #7799, .T. ) ;
#13085 = CARTESIAN_POINT ( 'NONE',  ( -21.50000000000000000, 2.999000000000001442, -52.50000000000000711 ) ) ;
#13086 = EDGE_LOOP ( 'NONE', ( #1073, #18654 ) ) ;
#13087 = ORIENTED_EDGE ( 'NONE', *, *, #8504, .F. ) ;
#13088 = EDGE_CURVE ( 'NONE', #19248, #2931, #13771, .T. ) ;
#13089 = CARTESIAN_POINT ( 'NONE',  ( -7.955834737091903364, -25.71081734191518464, 7.767572492083039570 ) ) ;
#13090 = VECTOR ( 'NONE', #1513, 1000.000000000000000 ) ;
#13091 = ORIENTED_EDGE ( 'NONE', *, *, #3396, .F. ) ;
#13093 = EDGE_LOOP ( 'NONE', ( #9096, #12577, #95, #14868, #10390 ) ) ;
#13092 = ORIENTED_EDGE ( 'NONE', *, *, #11178, .F. ) ;
#13094 = CARTESIAN_POINT ( 'NONE',  ( -17.51566270880199738, -25.64274437364856496, 41.23632249208304756 ) ) ;
#13095 = EDGE_CURVE ( 'NONE', #15143, #6791, #1159, .T. ) ;
#13096 = CARTESIAN_POINT ( 'NONE',  ( -9.020235676060220698, -27.64274437364852588, 32.26367750791695244 ) ) ;
#13097 = CIRCLE ( 'NONE', #13745, 2.999999999999999112 ) ;
#13098 = LINE ( 'NONE', #19295, #4771 ) ;
#13099 = CARTESIAN_POINT ( 'NONE',  ( 2.500000000000001776, 65.03553390593273775, 44.95000000218494307 ) ) ;
#13100 = LINE ( 'NONE', #5669, #3133 ) ;
#13101 = EDGE_LOOP ( 'NONE', ( #18714, #11430, #2783, #1149 ) ) ;
#13102 = CARTESIAN_POINT ( 'NONE',  ( -1.035533905932738863, 61.50000000000000000, 46.95000000000000284 ) ) ;
#13103 = ORIENTED_EDGE ( 'NONE', *, *, #6149, .F. ) ;
#13104 = ORIENTED_EDGE ( 'NONE', *, *, #19183, .T. ) ;
#13105 = DIRECTION ( 'NONE',  ( 0.000000000000000000, 0.000000000000000000, 1.000000000000000000 ) ) ;
#13106 = CARTESIAN_POINT ( 'NONE',  ( -41.00000000000000711, 110.0000000000000000, -11.50000000000000000 ) ) ;
#13107 = CARTESIAN_POINT ( 'NONE',  ( 24.99999999999998579, -6.000000000000000000, 47.49999999999997868 ) ) ;
#13108 = VECTOR ( 'NONE', #7306, 1000.000000000000000 ) ;
#13109 = CARTESIAN_POINT ( 'NONE',  ( 1.461580736456473906, 62.53841926354353120, 45.85000000109246798 ) ) ;
#13110 = EDGE_CURVE ( 'NONE', #10448, #3397, #8969, .T. ) ;
#13111 = CARTESIAN_POINT ( 'NONE',  ( -32.50000000000000000, 52.00000000000000711, 15.00000000000000000 ) ) ;
#13112 = VECTOR ( 'NONE', #15713, 1000.000000000000000 ) ;
#13113 = CARTESIAN_POINT ( 'NONE',  ( 1.035533905932739751, 61.50000000000000000, 47.15000000218494591 ) ) ;
#13114 = CIRCLE ( 'NONE', #4378, 2.649999999999999467 ) ;
#13115 = CARTESIAN_POINT ( 'NONE',  ( 4.999999999999999112, 0.000000000000000000, 0.000000000000000000 ) ) ;
#13116 = ORIENTED_EDGE ( 'NONE', *, *, #8690, .F. ) ;
#13118 = ORIENTED_EDGE ( 'NONE', *, *, #16957, .T. ) ;
#13117 = ORIENTED_EDGE ( 'NONE', *, *, #5296, .F. ) ;
#13119 = CARTESIAN_POINT ( 'NONE',  ( -7.955834737091916686, -22.28918265808470522, 5.357427507916955989 ) ) ;
#13120 = FACE_OUTER_BOUND ( 'NONE', #3949, .T. ) ;
#13121 = ORIENTED_EDGE ( 'NONE', *, *, #1876, .T. ) ;
#13122 = CARTESIAN_POINT ( 'NONE',  ( -17.99999999999999645, -24.16482700510260173, 4.923822492083043123 ) ) ;
#13123 = VECTOR ( 'NONE', #11749, 1000.000000000000000 ) ;
#13124 = LINE ( 'NONE', #1282, #1236 ) ;
#13125 = PRODUCT_RELATED_PRODUCT_CATEGORY ( 'part', '', ( #11758 ) ) ;
#13126 = ORIENTED_EDGE ( 'NONE', *, *, #11034, .T. ) ;
#13127 = CARTESIAN_POINT ( 'NONE',  ( -17.95583473709191580, -23.03132541760400898, 3.169927507916960874 ) ) ;
#13128 = VECTOR ( 'NONE', #9021, 1000.000000000000000 ) ;
#13129 = CARTESIAN_POINT ( 'NONE',  ( 2.500000000000001776, 64.00000000000000000, 48.79999999999999716 ) ) ;
#13130 = VERTEX_POINT ( 'NONE', #12000 ) ;
#13131 = CARTESIAN_POINT ( 'NONE',  ( 14.99999999999998579, 73.00000000000001421, 23.99999999999997158 ) ) ;
#13132 = ORIENTED_EDGE ( 'NONE', *, *, #1619, .T. ) ;
#13133 = CARTESIAN_POINT ( 'NONE',  ( -21.50000000000000000, 115.0000000000000000, 32.50000000000000000 ) ) ;
#13134 = DIRECTION ( 'NONE',  ( 0.5773502691896176264, -0.8164965809277319186, 0.000000000000000000 ) ) ;
#13135 = CARTESIAN_POINT ( 'NONE',  ( 3.000000000000000888, 0.000000000000000000, 0.000000000000000000 ) ) ;
#13136 = VECTOR ( 'NONE', #18908, 1000.000000000000000 ) ;
#13137 = EDGE_CURVE ( 'NONE', #15072, #10801, #4572, .T. ) ;
#13138 = APPLICATION_PROTOCOL_DEFINITION ( 'draft international standard', 'automotive_design', 1998, #2313 ) ;
#13139 = DIRECTION ( 'NONE',  ( -0.000000000000000000, 1.000000000000000000, -0.000000000000000000 ) ) ;
#13140 = CARTESIAN_POINT ( 'NONE',  ( -12.64274437364855252, -28.41254052147347053, 22.20117750791695599 ) ) ;
#13141 = CIRCLE ( 'NONE', #3768, 4.250000000000000000 ) ;
#13142 = LINE ( 'NONE', #5903, #5499 ) ;
#13143 = CARTESIAN_POINT ( 'NONE',  ( -17.64274437364855430, -28.24771351637087236, 2.076177507916958209 ) ) ;
#13144 = VECTOR ( 'NONE', #5399, 1000.000000000000000 ) ;
#13145 = DIRECTION ( 'NONE',  ( 0.7071067811865486830, 0.5000000000000005551, -0.4999999999999978351 ) ) ;
#13146 = ORIENTED_EDGE ( 'NONE', *, *, #526, .F. ) ;
#13147 = PRODUCT_DEFINITION_CONTEXT ( 'detailed design', #19088, 'design' ) ;
#13148 = CARTESIAN_POINT ( 'NONE',  ( -14.83517299489734853, -30.99999999999998224, 40.36132249208304046 ) ) ;
#13149 = CARTESIAN_POINT ( 'NONE',  ( -7.999999999999996447, -24.16482700510256976, 5.576177507916956877 ) ) ;
#13150 = CIRCLE ( 'NONE', #11277, 2.600000000000000089 ) ;
#13151 = CARTESIAN_POINT ( 'NONE',  ( -0.8561741729129461742, 66.06698729999999387, 46.20000000109247651 ) ) ;
#13152 = CARTESIAN_POINT ( 'NONE',  ( -17.68048971390462754, -22.64274437364856496, 5.361322492083044011 ) ) ;
#13153 = DIRECTION ( 'NONE',  ( 1.000000000000000000, 0.000000000000000000, 0.000000000000000000 ) ) ;
#13154 = EDGE_LOOP ( 'NONE', ( #265, #6263, #10963, #15455 ) ) ;
#13155 = AXIS2_PLACEMENT_3D ( 'NONE', #9413, #13831, #112 ) ;
#13156 = DIRECTION ( 'NONE',  ( 1.000000000000000000, -0.000000000000000000, -0.000000000000000000 ) ) ;
#13157 = CARTESIAN_POINT ( 'NONE',  ( -16.17491895705301275, -18.95583473709189803, 40.79492750791695954 ) ) ;
#13158 = CARTESIAN_POINT ( 'NONE',  ( 0.000000000000000000, 0.000000000000000000, 69.99999999999998579 ) ) ;
#13159 = DIRECTION ( 'NONE',  ( 1.000000000000000000, 0.000000000000000000, 0.000000000000000000 ) ) ;
#13160 = AXIS2_PLACEMENT_3D ( 'NONE', #8878, #16638, #8778 ) ;
#13161 = PLANE ( 'NONE',  #11858 ) ;
#13162 = CARTESIAN_POINT ( 'NONE',  ( -17.35725562635140307, -28.41254052147349185, 35.54882249208304046 ) ) ;
#13163 = CARTESIAN_POINT ( 'NONE',  ( 2.500000000000001776, 65.03553390593273775, 46.45000000000000284 ) ) ;
#13164 = CARTESIAN_POINT ( 'NONE',  ( -2.066987300000001415, 64.00000000000000000, 49.75000000109246656 ) ) ;
#13165 = VECTOR ( 'NONE', #1058, 1000.000000000000000 ) ;
#13166 = PRODUCT_DEFINITION_SHAPE ( 'NONE', 'NONE',  #19413 ) ;
#13167 = DIRECTION ( 'NONE',  ( 0.000000000000000000, 0.000000000000000000, -1.000000000000000000 ) ) ;
#13168 = CARTESIAN_POINT ( 'NONE',  ( -1.767766952966370209, 65.76776695296638309, 48.29999999999999716 ) ) ;
#13169 = DIRECTION ( 'NONE',  ( 0.000000000000000000, 0.000000000000000000, -1.000000000000000000 ) ) ;
#13170 = CIRCLE ( 'NONE', #3169, 2.499999999999998668 ) ;
#13171 = ORIENTED_EDGE ( 'NONE', *, *, #1921, .F. ) ;
#13172 = PRESENTATION_STYLE_ASSIGNMENT (( #8763 ) ) ;
#13173 = CARTESIAN_POINT ( 'NONE',  ( -9.955834737091912245, -22.82508104294696594, 10.60742750791695777 ) ) ;
#13174 = CARTESIAN_POINT ( 'NONE',  ( -13.64274437364856141, -26.68048971390460622, 37.95117750791695244 ) ) ;
#13175 = FACE_OUTER_BOUND ( 'NONE', #2253, .T. ) ;
#13176 = ADVANCED_FACE ( 'NONE', ( #3578 ), #6431, .F. ) ;
#13177 = CARTESIAN_POINT ( 'NONE',  ( -9.999999999999994671, -23.83517299489734143, 7.548822492083041347 ) ) ;
#13178 = VECTOR ( 'NONE', #5941, 1000.000000000000114 ) ;
#13179 = CARTESIAN_POINT ( 'NONE',  ( 2.066987300000001415, 64.00000000000000000, 46.95000000109246940 ) ) ;
#13180 = CARTESIAN_POINT ( 'NONE',  ( -16.64274437364856496, -26.51566270880199738, 38.82617750791695954 ) ) ;
#13181 = CARTESIAN_POINT ( 'NONE',  ( -13.82508104294698015, -29.04416526290806289, 6.669927507916956877 ) ) ;
#13182 = DIRECTION ( 'NONE',  ( 0.000000000000000000, 0.000000000000000000, -1.000000000000000000 ) ) ;
#13183 = AXIS2_PLACEMENT_3D ( 'NONE', #14566, #3700, #1138 ) ;
#13184 = FACE_OUTER_BOUND ( 'NONE', #9325, .T. ) ;
#13185 = DIRECTION ( 'NONE',  ( 0.000000000000000000, 0.000000000000000000, -1.000000000000000000 ) ) ;
#13186 = VECTOR ( 'NONE', #9958, 1000.000000000000000 ) ;
#13187 = CARTESIAN_POINT ( 'NONE',  ( -2.283493650000001818, 64.00000000000000000, 49.42500000163870766 ) ) ;
#13188 = CARTESIAN_POINT ( 'NONE',  ( 0.8561741729129471734, 61.93301270000000613, 48.40000000109247225 ) ) ;
#13189 = CARTESIAN_POINT ( 'NONE',  ( 1.300000000000000044, 0.7390083445627193548, -1.280000000000000693 ) ) ;
#13190 = EDGE_CURVE ( 'NONE', #1572, #1380, #15344, .T. ) ;
#13191 = DIRECTION ( 'NONE',  ( 0.000000000000000000, -0.7071067811865455743, -0.7071067811865495711 ) ) ;
#13192 = ORIENTED_EDGE ( 'NONE', *, *, #10576, .F. ) ;
#13193 = ORIENTED_EDGE ( 'NONE', *, *, #6762, .F. ) ;
#13194 = CARTESIAN_POINT ( 'NONE',  ( -9.996306089212364299, -29.24501739517662813, 37.73242750791695244 ) ) ;
#13195 = CARTESIAN_POINT ( 'NONE',  ( -15.16482700510263371, -18.99999999999997868, 0.9863224920830410136 ) ) ;
#13197 = ORIENTED_EDGE ( 'NONE', *, *, #8903, .T. ) ;
#13196 = VERTEX_POINT ( 'NONE', #4964 ) ;
#13198 = CARTESIAN_POINT ( 'NONE',  ( -12.04416526290807887, -24.96867458239596260, 0.5449275079169599856 ) ) ;
#13199 = CARTESIAN_POINT ( 'NONE',  ( -18.35725562635138886, -30.14459132904237393, 9.298822492083038682 ) ) ;
#13200 = CIRCLE ( 'NONE', #7270, 1.599999999999997202 ) ;
#13201 = DIRECTION ( 'NONE',  ( 0.000000000000000000, -1.000000000000000000, 0.000000000000000000 ) ) ;
#13202 = CARTESIAN_POINT ( 'NONE',  ( -1.461580736456473462, 62.53841926354353120, 48.85000000109246798 ) ) ;
#13203 = ORIENTED_EDGE ( 'NONE', *, *, #10465, .F. ) ;
#13204 = ORIENTED_EDGE ( 'NONE', *, *, #13553, .F. ) ;
#13205 = CARTESIAN_POINT ( 'NONE',  ( -2.500000000000001776, 64.00000000000000000, 46.79999999999999716 ) ) ;
#13206 = ORIENTED_EDGE ( 'NONE', *, *, #1942, .T. ) ;
#13207 = EDGE_CURVE ( 'NONE', #8594, #7260, #14252, .T. ) ;
#13208 = ADVANCED_FACE ( 'NONE', ( #823 ), #541, .T. ) ;
#13209 = EDGE_LOOP ( 'NONE', ( #16798, #8590, #9380 ) ) ;
#13210 = LINE ( 'NONE', #9266, #2562 ) ;
#13211 = PLANE ( 'NONE',  #19070 ) ;
#13212 = DIRECTION ( 'NONE',  ( 0.000000000000000000, 0.000000000000000000, 1.000000000000000000 ) ) ;
#13213 = EDGE_CURVE ( 'NONE', #89, #106, #18684, .T. ) ;
#13214 = CARTESIAN_POINT ( 'NONE',  ( 2.066987300000001859, 64.85617417291294373, 47.80000000109247082 ) ) ;
#13215 = CARTESIAN_POINT ( 'NONE',  ( -32.50000000000000000, 52.00000000000000711, -32.50000000000000000 ) ) ;
#13216 = CARTESIAN_POINT ( 'NONE',  ( 1.767766952966370653, 62.23223304703363112, 47.20000000218494307 ) ) ;
#13217 = CARTESIAN_POINT ( 'NONE',  ( 2.750000000000009770, 38.00000000000000000, -42.68883962248118991 ) ) ;
#13218 = EDGE_LOOP ( 'NONE', ( #7022, #8558, #11485, #18619 ) ) ;
#13220 = ORIENTED_EDGE ( 'NONE', *, *, #7374, .F. ) ;
#13219 = ORIENTED_EDGE ( 'NONE', *, *, #15264, .T. ) ;
#13221 = CARTESIAN_POINT ( 'NONE',  ( -14.83517299489740715, -16.99999999999997868, -0.9863224920830435671 ) ) ;
#13222 = CARTESIAN_POINT ( 'NONE',  ( 44.99999999999998579, 3.000000000000000000, -53.49999999999998579 ) ) ;
#13223 = VERTEX_POINT ( 'NONE', #18493 ) ;
#13224 = VERTEX_POINT ( 'NONE', #4866 ) ;
#13225 = CARTESIAN_POINT ( 'NONE',  ( -17.51566270880199738, -25.64274437364856496, 4.486322492083042235 ) ) ;
#13226 = CARTESIAN_POINT ( 'NONE',  ( -4.000000000000001776, 67.00000000000000000, 34.99999999999999289 ) ) ;
#13227 = EDGE_LOOP ( 'NONE', ( #16602, #10456, #8783, #17559 ) ) ;
#13228 = CARTESIAN_POINT ( 'NONE',  ( -11.99999999999999289, -24.16482700510258752, 0.3261775079169599856 ) ) ;
#13229 = DIRECTION ( 'NONE',  ( -1.156482317317871478E-16, 1.000000000000000000, 0.000000000000000000 ) ) ;
#13230 = VERTEX_POINT ( 'NONE', #18586 ) ;
#13231 = EDGE_CURVE ( 'NONE', #2845, #3455, #4219, .T. ) ;
#13232 = DIRECTION ( 'NONE',  ( 9.251858538542970348E-17, 0.000000000000000000, -1.000000000000000000 ) ) ;
#13233 = EDGE_LOOP ( 'NONE', ( #18955, #16214 ) ) ;
#13234 = CARTESIAN_POINT ( 'NONE',  ( -7.499999999999994671, -26.00000000000000355, 9.500000000000001776 ) ) ;
#13235 = FACE_OUTER_BOUND ( 'NONE', #17331, .T. ) ;
#13236 = LINE ( 'NONE', #5799, #5367 ) ;
#13237 = APPLICATION_PROTOCOL_DEFINITION ( 'draft international standard', 'automotive_design', 1998, #12696 ) ;
#13238 = CARTESIAN_POINT ( 'NONE',  ( -15.00000000000000000, 35.00000000000000000, 33.99999999999999289 ) ) ;
#13239 = CARTESIAN_POINT ( 'NONE',  ( -18.78091578003889950, -27.53959229564985378, 28.54492750791695954 ) ) ;
#13240 = CARTESIAN_POINT ( 'NONE',  ( -24.00000000000000711, 53.00000000000000711, 0.5000000000000004441 ) ) ;
#13241 = CARTESIAN_POINT ( 'NONE',  ( -18.53959229564986799, -20.21908421996107563, 8.857427507916957765 ) ) ;
#13242 = LINE ( 'NONE', #8934, #18685 ) ;
#13243 = VERTEX_POINT ( 'NONE', #15541 ) ;
#13244 = CARTESIAN_POINT ( 'NONE',  ( -18.64274437364860049, -18.02023567606023491, 42.54882249208304046 ) ) ;
#13245 = CARTESIAN_POINT ( 'NONE',  ( -7.955834737091916686, -22.28918265808470522, 5.357427507916955989 ) ) ;
#13246 = ADVANCED_FACE ( 'NONE', ( #637 ), #16921, .T. ) ;
#13247 = CARTESIAN_POINT ( 'NONE',  ( -1.461580736456473462, 62.53841926354353120, 44.85000000109246798 ) ) ;
#13248 = CARTESIAN_POINT ( 'NONE',  ( -16.17491895705296656, -29.04416526290807710, 40.58007249208304046 ) ) ;
#13249 = DIRECTION ( 'NONE',  ( -0.000000000000000000, -0.000000000000000000, -1.000000000000000000 ) ) ;
#13250 = ORIENTED_EDGE ( 'NONE', *, *, #10326, .T. ) ;
#13251 = CARTESIAN_POINT ( 'NONE',  ( -10.27562634311943057, -22.24032068463715106, -4.119453415227824499E-17 ) ) ;
#13252 = VERTEX_POINT ( 'NONE', #2298 ) ;
#13253 = CARTESIAN_POINT ( 'NONE',  ( -19.41254052147348830, -26.35725562635142083, 39.26367750791695954 ) ) ;
#13254 = DIRECTION ( 'NONE',  ( -1.000000000000000000, 0.000000000000000000, -7.304098846218135653E-17 ) ) ;
#13255 = CARTESIAN_POINT ( 'NONE',  ( 1.767766952966370653, 62.23223304703363112, 45.50000000000000000 ) ) ;
#13256 = CARTESIAN_POINT ( 'NONE',  ( -32.50000000000000000, 52.00000000000000711, 17.64999999999999858 ) ) ;
#13257 = CARTESIAN_POINT ( 'NONE',  ( -19.41254052147350961, -21.64274437364857562, 42.11132249208304046 ) ) ;
#13258 = EDGE_CURVE ( 'NONE', #16082, #11634, #14064, .T. ) ;
#13259 = CARTESIAN_POINT ( 'NONE',  ( -1.035533905932738863, 61.50000000000000000, 47.74999999999999289 ) ) ;
#13260 = CARTESIAN_POINT ( 'NONE',  ( -1.461580736456473906, 65.46158073645646880, 47.25000000109246656 ) ) ;
#13261 = CARTESIAN_POINT ( 'NONE',  ( -1.767766952966369765, 62.23223304703363112, 46.09999999999999432 ) ) ;
#13262 = CARTESIAN_POINT ( 'NONE',  ( -41.00000000000000711, 53.00000000000000711, -25.50000000000000000 ) ) ;
#13263 = ORIENTED_EDGE ( 'NONE', *, *, #4011, .F. ) ;
#13264 = CARTESIAN_POINT ( 'NONE',  ( -19.24771351637089367, -21.35725562635142438, 3.388677507916958653 ) ) ;
#13265 = EDGE_CURVE ( 'NONE', #19297, #9711, #5153, .T. ) ;
#13266 = CARTESIAN_POINT ( 'NONE',  ( -16.50457296725820555, -28.95583473709189448, 17.60742750791695599 ) ) ;
#13267 = DIRECTION ( 'NONE',  ( 0.000000000000000000, 0.000000000000000000, -1.000000000000000000 ) ) ;
#13268 = CARTESIAN_POINT ( 'NONE',  ( -16.50457296725825174, -19.04416526290807354, 6.017572492083042235 ) ) ;
#13269 = CARTESIAN_POINT ( 'NONE',  ( -0.8561741729129465073, 61.93301270000000613, 45.10000000109246798 ) ) ;
#13270 = CARTESIAN_POINT ( 'NONE',  ( -14.36097942780923731, -27.04416526290806999, 38.16992750791696665 ) ) ;
#13271 = CARTESIAN_POINT ( 'NONE',  ( -12.35725562635143682, -19.75228648362908501, 9.951177507916959541 ) ) ;
#13272 = CARTESIAN_POINT ( 'NONE',  ( -44.99999999999998579, -1.285879139104706187E-16, -56.59999999999999432 ) ) ;
#13273 = DIRECTION ( 'NONE',  ( -0.000000000000000000, -1.000000000000000000, -0.000000000000000000 ) ) ;
#13274 = CARTESIAN_POINT ( 'NONE',  ( 5.799999999999984723, 29.74264068711924835, 56.74264068711931230 ) ) ;
#13275 = STYLED_ITEM ( 'NONE', ( #18313 ), #18799 ) ;
#13276 = CARTESIAN_POINT ( 'NONE',  ( -1.040834085586084257E-14, 29.74264068711925901, 56.74264068711929809 ) ) ;
#13277 = VECTOR ( 'NONE', #7587, 1000.000000000000000 ) ;
#13278 = LINE ( 'NONE', #11811, #14609 ) ;
#13279 = FACE_OUTER_BOUND ( 'NONE', #6750, .T. ) ;
#13280 = CARTESIAN_POINT ( 'NONE',  ( -41.00000000000000711, 53.00000000000000711, 14.50000000000000000 ) ) ;
#13281 = ORIENTED_EDGE ( 'NONE', *, *, #18679, .T. ) ;
#13282 = VERTEX_POINT ( 'NONE', #733 ) ;
#13283 = CARTESIAN_POINT ( 'NONE',  ( -12.95952864787948755, -30.95583473709188382, 19.14257249208303691 ) ) ;
#13284 = FILL_AREA_STYLE_COLOUR ( '', #16189 ) ;
#13285 = DIRECTION ( 'NONE',  ( 1.000000000000000000, -0.000000000000000000, -0.000000000000000000 ) ) ;
#13287 = ORIENTED_EDGE ( 'NONE', *, *, #18855, .T. ) ;
#13286 = VERTEX_POINT ( 'NONE', #6527 ) ;
#13288 = CARTESIAN_POINT ( 'NONE',  ( -18.04416526290808775, -23.36097942780924441, 41.89257249208304046 ) ) ;
#13289 = CARTESIAN_POINT ( 'NONE',  ( 32.50000000000000000, -6.000000000000000000, -45.00000000000000000 ) ) ;
#13290 = CARTESIAN_POINT ( 'NONE',  ( -14.83517299489734853, -30.99999999999998224, 8.861322492083038682 ) ) ;
#13291 = AXIS2_PLACEMENT_3D ( 'NONE', #7434, #13402, #7637 ) ;
#13292 = VECTOR ( 'NONE', #8634, 1000.000000000000114 ) ;
#13293 = CARTESIAN_POINT ( 'NONE',  ( -3.065533689247737392, -46.96461745799954457, 1.500000000000000000 ) ) ;
#13294 = CARTESIAN_POINT ( 'NONE',  ( -2.500000000000001776, 65.03553390593273775, 44.45000000218495018 ) ) ;
#13295 = ORIENTED_EDGE ( 'NONE', *, *, #19263, .F. ) ;
#13296 = VERTEX_POINT ( 'NONE', #1923 ) ;
#13297 = EDGE_CURVE ( 'NONE', #3528, #4404, #2204, .T. ) ;
#13298 = ADVANCED_FACE ( 'NONE', ( #11114 ), #13967, .T. ) ;
#13299 = CARTESIAN_POINT ( 'NONE',  ( -25.00000000000000000, 110.0000000000000000, 30.00000000000000000 ) ) ;
#13300 = LINE ( 'NONE', #18124, #5108 ) ;
#13301 = VERTEX_POINT ( 'NONE', #12682 ) ;
#13302 = CARTESIAN_POINT ( 'NONE',  ( -2.750000000000019540, 115.0000000000000000, 37.49999999999997158 ) ) ;
#13303 = LINE ( 'NONE', #10462, #15334 ) ;
#13304 = ADVANCED_FACE ( 'NONE', ( #11202 ), #17021, .T. ) ;
#13305 = CARTESIAN_POINT ( 'NONE',  ( -2.066987300000001859, 64.85617417291294373, 48.10000000109246798 ) ) ;
#13306 = CARTESIAN_POINT ( 'NONE',  ( -1.040834085586084257E-14, 29.74264068711925901, 56.74264068711929809 ) ) ;
#13307 = AXIS2_PLACEMENT_3D ( 'NONE', #14030, #12272, #4739 ) ;
#13308 = AXIS2_PLACEMENT_3D ( 'NONE', #17734, #16639, #18106 ) ;
#13309 = FACE_OUTER_BOUND ( 'NONE', #8209, .T. ) ;
#13310 = ORIENTED_EDGE ( 'NONE', *, *, #18832, .F. ) ;
#13312 = VERTEX_POINT ( 'NONE', #9459 ) ;
#13311 = ORIENTED_EDGE ( 'NONE', *, *, #17882, .F. ) ;
#13313 = CARTESIAN_POINT ( 'NONE',  ( -8.855408670957631401, -20.64274437364852943, 20.88867750791695954 ) ) ;
#13314 = CARTESIAN_POINT ( 'NONE',  ( -40.00000000000000711, 110.0000000000000000, 30.00000000000000000 ) ) ;
#13315 = VERTEX_POINT ( 'NONE', #12491 ) ;
#13316 = ADVANCED_FACE ( 'NONE', ( #9744 ), #15736, .F. ) ;
#13317 = ORIENTED_EDGE ( 'NONE', *, *, #3894, .F. ) ;
#13318 = CARTESIAN_POINT ( 'NONE',  ( -13.35725562635141195, -26.51566270880198672, 3.173822492083044011 ) ) ;
#13319 = EDGE_CURVE ( 'NONE', #9095, #628, #4052, .T. ) ;
#13320 = DIRECTION ( 'NONE',  ( -0.000000000000000000, -0.000000000000000000, -1.000000000000000000 ) ) ;
#13321 = CARTESIAN_POINT ( 'NONE',  ( 2.500000000000001776, 64.00000000000000000, 47.30000000218494449 ) ) ;
#13322 = EDGE_LOOP ( 'NONE', ( #9112, #4518 ) ) ;
#13323 = CARTESIAN_POINT ( 'NONE',  ( -12.92450931948788906, -26.31681416490114245, 6.232427507916960430 ) ) ;
#13324 = AXIS2_PLACEMENT_3D ( 'NONE', #14473, #11421, #9676 ) ;
#13325 = CARTESIAN_POINT ( 'NONE',  ( -1.530808498934192803E-16, 66.50000000000000000, 47.50000000218494023 ) ) ;
#13326 = ORIENTED_EDGE ( 'NONE', *, *, #2336, .F. ) ;
#13327 = AXIS2_PLACEMENT_3D ( 'NONE', #11009, #6885, #14051 ) ;
#13328 = CARTESIAN_POINT ( 'NONE',  ( 1.300000000000000044, 1.478016689125442484, -1.626303258728256651E-15 ) ) ;
#13329 = PRODUCT_DEFINITION_SHAPE ( 'NONE', 'NONE',  #13627 ) ;
#13330 = ORIENTED_EDGE ( 'NONE', *, *, #19117, .T. ) ;
#13331 = EDGE_CURVE ( 'NONE', #3796, #4121, #916, .T. ) ;
#13332 = CARTESIAN_POINT ( 'NONE',  ( -25.00000000000000711, 53.00000000000000711, -6.000000000000001776 ) ) ;
#13333 = CARTESIAN_POINT ( 'NONE',  ( -50.00000000000002132, 33.00000000000000000, 59.99999999999997868 ) ) ;
#13334 = DIRECTION ( 'NONE',  ( 0.000000000000000000, 0.000000000000000000, 1.000000000000000000 ) ) ;
#13335 = APPLICATION_PROTOCOL_DEFINITION ( 'draft international standard', 'automotive_design', 1998, #2068 ) ;
#13336 = CARTESIAN_POINT ( 'NONE',  ( 43.50000000000001421, 2.999000000000001442, 32.49999999999998579 ) ) ;
#13337 = CARTESIAN_POINT ( 'NONE',  ( -1.530808498934192803E-16, 66.50000000000000000, 48.19999999999999574 ) ) ;
#13338 = CARTESIAN_POINT ( 'NONE',  ( -25.00000000000000000, 53.00000000000000711, 21.00000000000000000 ) ) ;
#13339 = CARTESIAN_POINT ( 'NONE',  ( -18.53959229564986799, -20.21908421996107563, 3.607427507916956877 ) ) ;
#13340 = VECTOR ( 'NONE', #11361, 1000.000000000000000 ) ;
#13341 = DIRECTION ( 'NONE',  ( 0.000000000000000000, 0.000000000000000000, 1.000000000000000000 ) ) ;
#13342 = EDGE_CURVE ( 'NONE', #17032, #12155, #14637, .T. ) ;
#13343 = EDGE_LOOP ( 'NONE', ( #2942, #7957, #19298, #8429 ) ) ;
#13344 = CONICAL_SURFACE ( 'NONE', #16163, 1.219500000000000028, 0.7853981633974680410 ) ;
#13345 = ADVANCED_FACE ( 'NONE', ( #17476 ), #5624, .F. ) ;
#13346 = PRODUCT_DEFINITION_CONTEXT ( 'detailed design', #14448, 'design' ) ;
#13347 = CARTESIAN_POINT ( 'NONE',  ( -18.78091578003892081, -20.46040770435013556, 5.580072492083041347 ) ) ;
#13348 = CARTESIAN_POINT ( 'NONE',  ( -12.95952864787955150, -17.04416526290805933, -0.7675724920830436782 ) ) ;
#13349 = CARTESIAN_POINT ( 'NONE',  ( 0.8561741729129472844, 61.93301270000000613, 45.00000000109246656 ) ) ;
#13350 = EDGE_CURVE ( 'NONE', #4393, #4220, #17386, .T. ) ;
#13351 = CARTESIAN_POINT ( 'NONE',  ( -17.07549068051208963, -26.31681416490115311, 4.267572492083044011 ) ) ;
#13352 = CARTESIAN_POINT ( 'NONE',  ( 1.035533905932738197, 66.50000000000000000, 45.75000000000000000 ) ) ;
#13353 = ORIENTED_EDGE ( 'NONE', *, *, #4629, .F. ) ;
#13354 = CARTESIAN_POINT ( 'NONE',  ( -12.14758986593398404, -18.81472126757313390, 5.414424919715185431E-14 ) ) ;
#13355 = VERTEX_POINT ( 'NONE', #7090 ) ;
#13356 = CARTESIAN_POINT ( 'NONE',  ( -19.24771351637089367, -21.35725562635142438, 40.13867750791695954 ) ) ;
#13357 = DIRECTION ( 'NONE',  ( -0.000000000000000000, -1.000000000000000000, -0.000000000000000000 ) ) ;
#13358 = AXIS2_PLACEMENT_3D ( 'NONE', #5983, #15101, #4516 ) ;
#13359 = CARTESIAN_POINT ( 'NONE',  ( 2.500000000000001776, 64.00000000000000000, 44.90000000218493881 ) ) ;
#13360 = CARTESIAN_POINT ( 'NONE',  ( -15.00000000000000000, 0.000000000000000000, 1.500000000000000444 ) ) ;
#13361 = CARTESIAN_POINT ( 'NONE',  ( 1.300000000000000044, -1.108512516844081475, 0.6400000000000016787 ) ) ;
#13362 = CARTESIAN_POINT ( 'NONE',  ( 0.8561741729129471734, 61.93301270000000613, 46.80000000109247082 ) ) ;
#13363 = ADVANCED_FACE ( 'NONE', ( #8375 ), #2772, .T. ) ;
#13364 =( NAMED_UNIT ( * ) SI_UNIT ( $, .STERADIAN. ) SOLID_ANGLE_UNIT ( ) );
#13365 = CARTESIAN_POINT ( 'NONE',  ( -2.500000000000000888, 62.96446609406726935, 47.64999999999999858 ) ) ;
#13366 = DIRECTION ( 'NONE',  ( -1.000000000000000000, 0.000000000000000000, -1.156482317317871725E-16 ) ) ;
#13367 = ORIENTED_EDGE ( 'NONE', *, *, #18679, .F. ) ;
#13368 =( LENGTH_UNIT ( ) NAMED_UNIT ( * ) SI_UNIT ( .MILLI., .METRE. ) );
#13369 = CARTESIAN_POINT ( 'NONE',  ( -13.82508104294698192, -29.04416526290806644, 1.419927507916958209 ) ) ;
#13370 = CARTESIAN_POINT ( 'NONE',  ( -18.53959229564986799, -20.21908421996107563, 14.10742750791695777 ) ) ;
#13371 = CARTESIAN_POINT ( 'NONE',  ( -0.3715438340500360481, 66.44684080192190834, 45.00000000000000711 ) ) ;
#13372 = CARTESIAN_POINT ( 'NONE',  ( -13.49542703274174116, -28.95583473709188738, 8.642572492083040459 ) ) ;
#13373 = CARTESIAN_POINT ( 'NONE',  ( 1.461580736456473906, 62.53841926354353120, 46.05000000109246372 ) ) ;
#13374 = CARTESIAN_POINT ( 'NONE',  ( -16.17491895705301275, -18.95583473709189803, 4.044927507916959541 ) ) ;
#13375 = LINE ( 'NONE', #7136, #5631 ) ;
#13376 = LINE ( 'NONE', #17698, #6600 ) ;
#13377 = CARTESIAN_POINT ( 'NONE',  ( -4.012354697599906928, 32.70432772728319293, 53.78000129688592068 ) ) ;
#13378 = DIRECTION ( 'NONE',  ( 0.000000000000000000, 0.000000000000000000, -1.000000000000000000 ) ) ;
#13379 = LINE ( 'NONE', #8774, #5901 ) ;
#13380 = CARTESIAN_POINT ( 'NONE',  ( 24.00000000000000000, 47.00000000000000711, 18.00000000000000000 ) ) ;
#13381 = DIRECTION ( 'NONE',  ( 0.000000000000000000, 0.000000000000000000, -1.000000000000000000 ) ) ;
#13382 = DIRECTION ( 'NONE',  ( 0.000000000000000000, -1.000000000000000000, 0.000000000000000000 ) ) ;
#13383 = FACE_OUTER_BOUND ( 'NONE', #5999, .T. ) ;
#13384 = VERTEX_POINT ( 'NONE', #7184 ) ;
#13385 = VERTEX_POINT ( 'NONE', #19052 ) ;
#13386 = CARTESIAN_POINT ( 'NONE',  ( -11.35725562635139418, -29.97976432393972601, 13.67382249208304046 ) ) ;
#13387 = CARTESIAN_POINT ( 'NONE',  ( -41.00000000000000711, 53.00000000000000711, 13.50000000000000000 ) ) ;
#13389 = ORIENTED_EDGE ( 'NONE', *, *, #2199, .F. ) ;
#13388 = VERTEX_POINT ( 'NONE', #4254 ) ;
#13390 = CARTESIAN_POINT ( 'NONE',  ( -13.35725562635142794, -21.48433729119796709, 20.45117750791696309 ) ) ;
#13391 = DIRECTION ( 'NONE',  ( -2.220446049250312588E-16, 0.7071067811865453523, 0.7071067811865496822 ) ) ;
#13392 = CARTESIAN_POINT ( 'NONE',  ( -18.64274437364860049, -18.02023567606023491, 5.798822492083038682 ) ) ;
#13393 = CARTESIAN_POINT ( 'NONE',  ( 1.461580736456473684, 65.46158073645646880, 48.45000000109247651 ) ) ;
#13394 = CARTESIAN_POINT ( 'NONE',  ( 1.035533905932738197, 66.50000000000000000, 45.85000000218494165 ) ) ;
#13395 = EDGE_LOOP ( 'NONE', ( #4136, #11149, #18169, #12905 ) ) ;
#13396 = ORIENTED_EDGE ( 'NONE', *, *, #5566, .T. ) ;
#13397 = VECTOR ( 'NONE', #1727, 1000.000000000000000 ) ;
#13398 = CARTESIAN_POINT ( 'NONE',  ( -2.500000000000001776, 62.96446609406726225, 46.84999999999998721 ) ) ;
#13399 = FACE_OUTER_BOUND ( 'NONE', #938, .T. ) ;
#13400 = EDGE_LOOP ( 'NONE', ( #2270, #6648 ) ) ;
#13401 = DIRECTION ( 'NONE',  ( 0.000000000000000000, 0.000000000000000000, 1.000000000000000000 ) ) ;
#13402 = DIRECTION ( 'NONE',  ( -0.7071067811865390240, 0.5000000000000073275, -0.5000000000000048850 ) ) ;
#13403 = CARTESIAN_POINT ( 'NONE',  ( 1.461580736456473906, 62.53841926354353120, 47.65000000109247225 ) ) ;
#13404 = PLANE ( 'NONE',  #4407 ) ;
#13405 = DIRECTION ( 'NONE',  ( 0.000000000000000000, 0.000000000000000000, -1.000000000000000000 ) ) ;
#13406 = ORIENTED_EDGE ( 'NONE', *, *, #2246, .F. ) ;
#13408 = ORIENTED_EDGE ( 'NONE', *, *, #16636, .T. ) ;
#13407 = VERTEX_POINT ( 'NONE', #6899 ) ;
#13409 = ADVANCED_FACE ( 'NONE', ( #17677 ), #16021, .F. ) ;
#13410 = CARTESIAN_POINT ( 'NONE',  ( -20.97976432393977575, -20.35725562635143504, 19.13867750791695954 ) ) ;
#13411 = VECTOR ( 'NONE', #6995, 1000.000000000000227 ) ;
#13412 = LINE ( 'NONE', #8821, #6173 ) ;
#13413 = ORIENTED_EDGE ( 'NONE', *, *, #6863, .T. ) ;
#13414 = ORIENTED_EDGE ( 'NONE', *, *, #10430, .F. ) ;
#13415 = CARTESIAN_POINT ( 'NONE',  ( -12.31951028609536536, -25.35725562635139596, 23.73632249208304401 ) ) ;
#13416 = EDGE_CURVE ( 'NONE', #7552, #10804, #1019, .T. ) ;
#13417 = DIRECTION ( 'NONE',  ( 0.000000000000000000, 0.000000000000000000, -1.000000000000000000 ) ) ;
#13418 = DIRECTION ( 'NONE',  ( 0.000000000000000000, -0.6139406135149196864, 0.7893522173763268812 ) ) ;
#13419 = ORIENTED_EDGE ( 'NONE', *, *, #16305, .F. ) ;
#13420 = CARTESIAN_POINT ( 'NONE',  ( -17.99999999999999645, -23.83517299489736985, 2.951177507916960430 ) ) ;
#13421 = EDGE_CURVE ( 'NONE', #10089, #7522, #5340, .T. ) ;
#13422 = VECTOR ( 'NONE', #4480, 1000.000000000000000 ) ;
#13423 = FACE_OUTER_BOUND ( 'NONE', #7919, .T. ) ;
#13424 = EDGE_LOOP ( 'NONE', ( #17421, #17351, #5205 ) ) ;
#13425 = DIRECTION ( 'NONE',  ( -1.000000000000000000, 0.000000000000000000, -9.251858538542970348E-17 ) ) ;
#13426 = ORIENTED_EDGE ( 'NONE', *, *, #18361, .T. ) ;
#13427 = DIRECTION ( 'NONE',  ( -1.156482317317871478E-16, 1.000000000000000000, 0.000000000000000000 ) ) ;
#13428 = DIRECTION ( 'NONE',  ( -2.168404344971008868E-16, 1.000000000000000000, 0.000000000000000000 ) ) ;
#13429 = LINE ( 'NONE', #11762, #5984 ) ;
#13430 = VECTOR ( 'NONE', #5973, 1000.000000000000000 ) ;
#13431 = APPLICATION_PROTOCOL_DEFINITION ( 'draft international standard', 'automotive_design', 1998, #2679 ) ;
#13432 = DIRECTION ( 'NONE',  ( 0.000000000000000000, 0.000000000000000000, -1.000000000000000000 ) ) ;
#13433 = CARTESIAN_POINT ( 'NONE',  ( -19.41254052147348830, -26.35725562635142083, 39.26367750791695954 ) ) ;
#13434 = DIRECTION ( 'NONE',  ( -1.000000000000000000, 0.000000000000000000, -0.000000000000000000 ) ) ;
#13435 = EDGE_CURVE ( 'NONE', #16948, #10054, #8560, .T. ) ;
#13436 = CARTESIAN_POINT ( 'NONE',  ( -15.16482700510259640, -28.99999999999998224, 17.38867750791695599 ) ) ;
#13437 = VECTOR ( 'NONE', #2642, 1000.000000000000000 ) ;
#13438 = CARTESIAN_POINT ( 'NONE',  ( -3.155775640247338920, -38.39960408384397539, 1.500000000000000000 ) ) ;
#13439 = VERTEX_POINT ( 'NONE', #17585 ) ;
#13440 = CARTESIAN_POINT ( 'NONE',  ( -18.78091578003892081, -20.46040770435013556, 21.33007249208303691 ) ) ;
#13441 = APPLICATION_CONTEXT ( 'automotive_design' ) ;
#13442 = VECTOR ( 'NONE', #2966, 1000.000000000000000 ) ;
#13443 = CIRCLE ( 'NONE', #3446, 2.999999999999999112 ) ;
#13444 = CARTESIAN_POINT ( 'NONE',  ( 1.461580736456473684, 65.46158073645646880, 45.25000000109247367 ) ) ;
#13445 = CARTESIAN_POINT ( 'NONE',  ( -12.92450931948790149, -21.68318583509881137, 6.892572492083043123 ) ) ;
#13446 = LINE ( 'NONE', #30, #14729 ) ;
#13447 = ORIENTED_EDGE ( 'NONE', *, *, #19188, .F. ) ;
#13448 = VECTOR ( 'NONE', #491, 1000.000000000000000 ) ;
#13449 = LINE ( 'NONE', #10210, #1563 ) ;
#13450 = ORIENTED_EDGE ( 'NONE', *, *, #15362, .F. ) ;
#13451 = CARTESIAN_POINT ( 'NONE',  ( 14.99999999999998579, 73.00000000000001421, 20.99999999999997513 ) ) ;
#13452 = CARTESIAN_POINT ( 'NONE',  ( -32.50000000000000000, 52.00000000000000711, -32.50000000000000000 ) ) ;
#13453 = DIRECTION ( 'NONE',  ( -1.000000000000000000, -0.000000000000000000, -0.000000000000000000 ) ) ;
#13454 = DIRECTION ( 'NONE',  ( 0.000000000000000000, -1.000000000000000000, 0.000000000000000000 ) ) ;
#13455 = EDGE_CURVE ( 'NONE', #9088, #8057, #18959, .T. ) ;
#13456 = EDGE_CURVE ( 'NONE', #4041, #7547, #5164, .T. ) ;
#13457 = VECTOR ( 'NONE', #17477, 1000.000000000000000 ) ;
#13458 = CARTESIAN_POINT ( 'NONE',  ( 0.8561741729129471734, 61.93301270000000613, 48.40000000109247225 ) ) ;
#13459 = EDGE_CURVE ( 'NONE', #1673, #9439, #11684, .T. ) ;
#13460 = CIRCLE ( 'NONE', #936, 4.000000000000001776 ) ;
#13461 = B_SPLINE_CURVE_WITH_KNOTS ( 'NONE', 3,
 ( #13005, #11248, #4106, #5476 ),
 .UNSPECIFIED., .F., .F.,
 ( 4, 4 ),
 ( 0.000000000000000000, 1.000000000000000000 ),
 .UNSPECIFIED. ) ;
#13462 = DIRECTION ( 'NONE',  ( 0.000000000000000000, -0.000000000000000000, 1.000000000000000000 ) ) ;
#13463 = CARTESIAN_POINT ( 'NONE',  ( 1.767766952966369987, 65.76776695296638309, 48.09999999999999432 ) ) ;
#13464 = CARTESIAN_POINT ( 'NONE',  ( 3.399999999999996803, 29.65425233947092920, 56.47747564417434774 ) ) ;
#13465 = CIRCLE ( 'NONE', #10649, 2.700000000000000622 ) ;
#13466 = VERTEX_POINT ( 'NONE', #11303 ) ;
#13467 = DIRECTION ( 'NONE',  ( 0.000000000000000000, 0.000000000000000000, 1.000000000000000000 ) ) ;
#13468 = VECTOR ( 'NONE', #11563, 1000.000000000000000 ) ;
#13469 = CARTESIAN_POINT ( 'NONE',  ( -11.21908421996108629, -20.46040770435011069, 4.919927507916955989 ) ) ;
#13470 = CARTESIAN_POINT ( 'NONE',  ( -17.64274437364855430, -28.24771351637087236, 17.82617750791695599 ) ) ;
#13471 = CARTESIAN_POINT ( 'NONE',  ( -1.749252862646410556, 65.52426609366526122, 45.00000000000003553 ) ) ;
#13472 = CARTESIAN_POINT ( 'NONE',  ( -19.24771351637086880, -26.64274437364857206, 9.736322492083042235 ) ) ;
#13473 = VECTOR ( 'NONE', #9516, 1000.000000000000000 ) ;
#13474 = CARTESIAN_POINT ( 'NONE',  ( -1.461580736456473906, 65.46158073645646880, 44.85000000109246798 ) ) ;
#13475 = EDGE_CURVE ( 'NONE', #17318, #17032, #3959, .T. ) ;
#13476 = CARTESIAN_POINT ( 'NONE',  ( -16.35725562635142794, -21.31951028609535470, 40.57617750791696665 ) ) ;
#13477 = ADVANCED_FACE ( 'NONE', ( #4161 ), #10112, .F. ) ;
#13478 = CARTESIAN_POINT ( 'NONE',  ( 2.500000000000000000, 2.357898499370431722, -2.818925648462311528E-15 ) ) ;
#13479 = CARTESIAN_POINT ( 'NONE',  ( -10.75228648362910100, -26.64274437364854009, 6.013677507916958653 ) ) ;
#13480 = DIRECTION ( 'NONE',  ( -1.541976423090495880E-16, 0.000000000000000000, 1.000000000000000000 ) ) ;
#13481 = PRESENTATION_LAYER_ASSIGNMENT (  '', '', ( #5977 ) ) ;
#13482 = CARTESIAN_POINT ( 'NONE',  ( -41.00000000000000711, 53.00000000000000711, 20.00000000000000000 ) ) ;
#13483 = LINE ( 'NONE', #3091, #7504 ) ;
#13484 = CARTESIAN_POINT ( 'NONE',  ( 1.767766952966369987, 65.76776695296638309, 49.69999999999999574 ) ) ;
#13485 = AXIS2_PLACEMENT_3D ( 'NONE', #4899, #9577, #15571 ) ;
#13486 = CARTESIAN_POINT ( 'NONE',  ( 1.461580736456473906, 62.53841926354353120, 46.05000000109246372 ) ) ;
#13487 = CARTESIAN_POINT ( 'NONE',  ( -25.00000000000000000, 53.00000000000000711, 30.00000000000000000 ) ) ;
#13488 = VECTOR ( 'NONE', #6050, 1000.000000000000000 ) ;
#13489 = LINE ( 'NONE', #11010, #7390 ) ;
#13490 = EDGE_LOOP ( 'NONE', ( #9528, #10167 ) ) ;
#13491 = VERTEX_POINT ( 'NONE', #2388 ) ;
#13492 = CARTESIAN_POINT ( 'NONE',  ( -20.24501739517669563, -18.99630608921239627, 21.33007249208303691 ) ) ;
#13493 = FACE_OUTER_BOUND ( 'NONE', #1181, .T. ) ;
#13495 = ORIENTED_EDGE ( 'NONE', *, *, #16313, .T. ) ;
#13494 = ORIENTED_EDGE ( 'NONE', *, *, #14904, .F. ) ;
#13496 = PRODUCT_DEFINITION_SHAPE ( 'NONE', 'NONE',  #19405 ) ;
#13497 = CARTESIAN_POINT ( 'NONE',  ( -17.31681416490115311, -26.07549068051209318, 18.04492750791696309 ) ) ;
#13498 = CARTESIAN_POINT ( 'NONE',  ( 2.499999999999996003, 62.96446609406726225, 48.85000000218494165 ) ) ;
#13499 = CARTESIAN_POINT ( 'NONE',  ( -16.71081734191520596, -31.04416526290808065, 3.830072492083039126 ) ) ;
#13500 = AXIS2_PLACEMENT_3D ( 'NONE', #19179, #4382, #17806 ) ;
#13501 = CARTESIAN_POINT ( 'NONE',  ( -1.530808498934192803E-16, 66.50000000000000000, 45.00000000000000000 ) ) ;
#13502 = CARTESIAN_POINT ( 'NONE',  ( 1.461580736456473684, 65.46158073645646880, 49.25000000109246656 ) ) ;
#13503 = VERTEX_POINT ( 'NONE', #14344 ) ;
#13504 = EDGE_CURVE ( 'NONE', #9977, #834, #15917, .T. ) ;
#13505 = VERTEX_POINT ( 'NONE', #234 ) ;
#13506 = AXIS2_PLACEMENT_3D ( 'NONE', #3247, #2160, #11073 ) ;
#13507 = DIRECTION ( 'NONE',  ( -0.7071067811865487940, -0.5000000000000003331, 0.4999999999999979461 ) ) ;
#13508 = CARTESIAN_POINT ( 'NONE',  ( -5.800000000000006928, 29.47747564417435484, 56.65425233947093631 ) ) ;
#13509 = EDGE_LOOP ( 'NONE', ( #14144, #6373, #7952, #15522 ) ) ;
#13510 = CARTESIAN_POINT ( 'NONE',  ( -3.065533689247737392, -45.28611686177728046, 1.500000000000000000 ) ) ;
#13511 = CARTESIAN_POINT ( 'NONE',  ( -41.00000000000000711, 53.00000000000000711, 8.000000000000000000 ) ) ;
#13512 = CARTESIAN_POINT ( 'NONE',  ( -0.8561741729129465073, 61.93301270000000613, 48.30000000109247082 ) ) ;
#13513 = DIRECTION ( 'NONE',  ( 0.000000000000000000, 0.000000000000000000, 1.000000000000000000 ) ) ;
#13514 = VECTOR ( 'NONE', #7665, 1000.000000000000000 ) ;
#13515 = CARTESIAN_POINT ( 'NONE',  ( 3.999999999999998224, 67.00000000000000000, 30.00000000000000000 ) ) ;
#13516 = VERTEX_POINT ( 'NONE', #16507 ) ;
#13518 = ORIENTED_EDGE ( 'NONE', *, *, #17427, .F. ) ;
#13517 = ORIENTED_EDGE ( 'NONE', *, *, #17527, .T. ) ;
#13519 = CARTESIAN_POINT ( 'NONE',  ( -16.71081734191527346, -16.95583473709190159, 14.54492750791695421 ) ) ;
#13520 = AXIS2_PLACEMENT_3D ( 'NONE', #3196, #4304, #10262 ) ;
#13521 = PLANE ( 'NONE',  #17124 ) ;
#13522 = VERTEX_POINT ( 'NONE', #11886 ) ;
#13523 = ORIENTED_EDGE ( 'NONE', *, *, #13010, .T. ) ;
#13524 = CARTESIAN_POINT ( 'NONE',  ( -17.68048971390462754, -22.64274437364856496, 21.11132249208304401 ) ) ;
#13525 = EDGE_CURVE ( 'NONE', #2239, #6673, #3173, .T. ) ;
#13526 = CARTESIAN_POINT ( 'NONE',  ( -2.500000000000001776, 64.00000000000000000, 45.19999999999999574 ) ) ;
#13527 = DIRECTION ( 'NONE',  ( -0.000000000000000000, 1.000000000000000000, -0.000000000000000000 ) ) ;
#13528 = ADVANCED_FACE ( 'NONE', ( #1612 ), #17777, .F. ) ;
#13529 = ORIENTED_EDGE ( 'NONE', *, *, #15515, .F. ) ;
#13530 = CARTESIAN_POINT ( 'NONE',  ( -14.03132541760401786, -21.04416526290806289, 14.98242750791695954 ) ) ;
#13531 = CARTESIAN_POINT ( 'NONE',  ( -40.00000000000000711, 110.0000000000000000, 6.999999999999999112 ) ) ;
#13532 = ORIENTED_EDGE ( 'NONE', *, *, #4473, .T. ) ;
#13533 = CARTESIAN_POINT ( 'NONE',  ( 49.99999999999998579, 3.000000000000000000, 59.99999999999997868 ) ) ;
#13534 = EDGE_LOOP ( 'NONE', ( #1842, #5571, #11658, #8416, #19210, #16072, #1972, #2193 ) ) ;
#13535 = LINE ( 'NONE', #16876, #12540 ) ;
#13536 = CYLINDRICAL_SURFACE ( 'NONE', #8929, 2.500000000000001776 ) ;
#13537 = CARTESIAN_POINT ( 'NONE',  ( -9.120482147295685276E-15, 33.84386001800124433, 52.64142135623733054 ) ) ;
#13538 = APPLICATION_PROTOCOL_DEFINITION ( 'draft international standard', 'automotive_design', 1998, #15093 ) ;
#13539 = CARTESIAN_POINT ( 'NONE',  ( -41.00000000000000711, 53.00000000000000711, -12.50000000000000000 ) ) ;
#13540 = CARTESIAN_POINT ( 'NONE',  ( 1.767766952966369987, 65.76776695296638309, 48.09999999999999432 ) ) ;
#13541 = LINE ( 'NONE', #13338, #16461 ) ;
#13542 = CARTESIAN_POINT ( 'NONE',  ( -10.75228648362910100, -26.64274437364854009, 11.26367750791695777 ) ) ;
#13543 = DIRECTION ( 'NONE',  ( 0.000000000000000000, 0.000000000000000000, 1.000000000000000000 ) ) ;
#13544 = VERTEX_POINT ( 'NONE', #4355 ) ;
#13545 = CARTESIAN_POINT ( 'NONE',  ( -10.04416526290808953, -22.49542703274172695, 23.08007249208303335 ) ) ;
#13546 = CARTESIAN_POINT ( 'NONE',  ( 4.042620306204079306, 32.68389060951040648, 53.80012125920699617 ) ) ;
#13547 = CARTESIAN_POINT ( 'NONE',  ( -15.16482700510262482, -20.99999999999997513, 16.73632249208304046 ) ) ;
#13548 = CARTESIAN_POINT ( 'NONE',  ( -2.500000000000006661, 65.03553390593272354, 45.94999999999999574 ) ) ;
#13549 = VERTEX_POINT ( 'NONE', #13452 ) ;
#13550 = CARTESIAN_POINT ( 'NONE',  ( -10.37592340745185382, -20.82129991144855907, 3.747711961066386859E-16 ) ) ;
#13551 = ORIENTED_EDGE ( 'NONE', *, *, #12564, .T. ) ;
#13552 = CARTESIAN_POINT ( 'NONE',  ( 4.101219330881969327, 32.64264068711926825, 53.84264068711931372 ) ) ;
#13553 = EDGE_CURVE ( 'NONE', #2359, #10684, #1512, .T. ) ;
#13554 = LINE ( 'NONE', #16306, #18939 ) ;
#13555 = CARTESIAN_POINT ( 'NONE',  ( 0.000000000000000000, 52.00000000000000711, -67.72004514666936359 ) ) ;
#13556 = DIRECTION ( 'NONE',  ( -1.156482317317871478E-16, 1.000000000000000000, 0.000000000000000000 ) ) ;
#13557 = CARTESIAN_POINT ( 'NONE',  ( -2.066987300000001415, 64.00000000000000000, 46.55000000109247082 ) ) ;
#13558 = FILL_AREA_STYLE ('',( #17982 ) ) ;
#13559 = CARTESIAN_POINT ( 'NONE',  ( -2.500000000000001776, 65.03553390593273775, 47.54999999999999716 ) ) ;
#13560 = DIRECTION ( 'NONE',  ( -0.000000000000000000, -1.000000000000000000, -0.000000000000000000 ) ) ;
#13561 = VERTEX_POINT ( 'NONE', #12082 ) ;
#13562 = CARTESIAN_POINT ( 'NONE',  ( 0.000000000000000000, 0.000000000000000000, 0.000000000000000000 ) ) ;
#13563 = CARTESIAN_POINT ( 'NONE',  ( -14.83517299489739649, -18.99999999999997868, 14.76367750791695777 ) ) ;
#13564 = EDGE_CURVE ( 'NONE', #11844, #4857, #3274, .T. ) ;
#13565 = CARTESIAN_POINT ( 'NONE',  ( -12.35725562635143682, -19.75228648362908501, 15.20117750791695777 ) ) ;
#13566 = CARTESIAN_POINT ( 'NONE',  ( 1.035533905932738197, 66.50000000000000000, 49.05000000218495160 ) ) ;
#13567 = EDGE_CURVE ( 'NONE', #18422, #1873, #9535, .T. ) ;
#13568 = CARTESIAN_POINT ( 'NONE',  ( -17.64274437364858983, -19.75228648362910633, 5.798822492083041347 ) ) ;
#13569 = CARTESIAN_POINT ( 'NONE',  ( -24.00000000000000000, 110.0000000000000000, 30.00000000000000000 ) ) ;
#13570 = CARTESIAN_POINT ( 'NONE',  ( -12.35725562635143682, -19.75228648362908501, -0.5488224920830419018 ) ) ;
#13571 = CARTESIAN_POINT ( 'NONE',  ( 43.50000000000001421, 2.999000000000001442, 32.49999999999998579 ) ) ;
#13572 = CARTESIAN_POINT ( 'NONE',  ( -18.53959229564986799, -20.21908421996107563, 24.60742750791695954 ) ) ;
#13573 = LINE ( 'NONE', #12002, #17199 ) ;
#13574 = FACE_OUTER_BOUND ( 'NONE', #15421, .T. ) ;
#13575 = CARTESIAN_POINT ( 'NONE',  ( -0.8561741729129465073, 61.93301270000000613, 46.70000000109248361 ) ) ;
#13576 = CARTESIAN_POINT ( 'NONE',  ( -32.50000000000001421, -6.000000000000000000, 44.99999999999997868 ) ) ;
#13577 = LINE ( 'NONE', #16528, #5070 ) ;
#13578 = CARTESIAN_POINT ( 'NONE',  ( 0.8561741729129460632, 66.06698730000000808, 45.50000000109247367 ) ) ;
#13579 = FACE_OUTER_BOUND ( 'NONE', #14317, .T. ) ;
#13580 = LINE ( 'NONE', #7713, #8938 ) ;
#13581 = VECTOR ( 'NONE', #16286, 1000.000000000000000 ) ;
#13582 = DIRECTION ( 'NONE',  ( 0.000000000000000000, -0.7071067811865457964, -0.7071067811865492381 ) ) ;
#13583 = EDGE_LOOP ( 'NONE', ( #195, #6284, #8907, #2839, #11559, #3420 ) ) ;
#13584 = EDGE_LOOP ( 'NONE', ( #6847, #6057, #18738, #5819 ) ) ;
#13585 = CARTESIAN_POINT ( 'NONE',  ( -18.35725562635138886, -30.14459132904237393, 25.04882249208303691 ) ) ;
#13586 = EDGE_CURVE ( 'NONE', #4916, #9301, #13554, .T. ) ;
#13587 = DIRECTION ( 'NONE',  ( 0.000000000000000000, -0.000000000000000000, -1.000000000000000000 ) ) ;
#13589 = ORIENTED_EDGE ( 'NONE', *, *, #11976, .T. ) ;
#13588 = EDGE_LOOP ( 'NONE', ( #11979, #8816, #10585, #13126 ) ) ;
#13590 = CARTESIAN_POINT ( 'NONE',  ( -17.07549068051210739, -21.68318583509881847, 8.857427507916959541 ) ) ;
#13591 = CARTESIAN_POINT ( 'NONE',  ( -41.00000000000000000, 52.00000000000000711, -67.72004514666936359 ) ) ;
#13592 = CARTESIAN_POINT ( 'NONE',  ( -8.044165262908093084, -21.95952864787946979, 2.080072492083039126 ) ) ;
#13593 = CARTESIAN_POINT ( 'NONE',  ( -2.749999999999988454, 37.99999999999999289, 40.49999999999996447 ) ) ;
#13594 = CARTESIAN_POINT ( 'NONE',  ( -0.8561741729129461742, 66.06698729999999387, 47.80000000109247082 ) ) ;
#13595 = ORIENTED_EDGE ( 'NONE', *, *, #12470, .T. ) ;
#13596 = ORIENTED_EDGE ( 'NONE', *, *, #11069, .F. ) ;
#13597 = EDGE_CURVE ( 'NONE', #6401, #9098, #9150, .T. ) ;
#13598 = STYLED_ITEM ( 'NONE', ( #17712 ), #12712 ) ;
#13599 = CARTESIAN_POINT ( 'NONE',  ( 41.99999999999997868, 6.000000000000005329, 51.99999999999997868 ) ) ;
#13600 = LINE ( 'NONE', #8896, #10039 ) ;
#13601 = AXIS2_PLACEMENT_3D ( 'NONE', #10018, #5436, #14444 ) ;
#13602 = VERTEX_POINT ( 'NONE', #7385 ) ;
#13603 = CARTESIAN_POINT ( 'NONE',  ( -10.57758699569699523, -22.20123138602766133, 1.196196559315024355E-16 ) ) ;
#13604 = PLANE ( 'NONE',  #4044 ) ;
#13605 = CARTESIAN_POINT ( 'NONE',  ( 1.461580736456473684, 65.46158073645646880, 46.25000000109246656 ) ) ;
#13606 = CARTESIAN_POINT ( 'NONE',  ( -41.00000000000000711, 110.0000000000000000, 1.500000000000001332 ) ) ;
#13607 = DIRECTION ( 'NONE',  ( -0.000000000000000000, -0.000000000000000000, -1.000000000000000000 ) ) ;
#13608 = ADVANCED_FACE ( 'NONE', ( #6118 ), #18081, .T. ) ;
#13609 = ORIENTED_EDGE ( 'NONE', *, *, #6149, .T. ) ;
#13611 = ORIENTED_EDGE ( 'NONE', *, *, #18567, .F. ) ;
#13610 = ORIENTED_EDGE ( 'NONE', *, *, #15020, .T. ) ;
#13612 = CARTESIAN_POINT ( 'NONE',  ( -20.24501739517664234, -29.00369391078761439, 12.79492750791695599 ) ) ;
#13613 = VERTEX_POINT ( 'NONE', #15035 ) ;
#13614 = AXIS2_PLACEMENT_3D ( 'NONE', #9335, #15433, #12472 ) ;
#13615 = ORIENTED_EDGE ( 'NONE', *, *, #7515, .T. ) ;
#13616 = CARTESIAN_POINT ( 'NONE',  ( -16.35725562635141372, -26.68048971390461332, 19.79882249208304046 ) ) ;
#13617 =( BOUNDED_CURVE ( )  B_SPLINE_CURVE ( 2, ( #17953, #1285, #18054, #10483, #13325, #108, #7262, #4324, #12055 ),
 .UNSPECIFIED., .F., .F. ) 
 B_SPLINE_CURVE_WITH_KNOTS ( ( 3, 2, 2, 2, 3 ),
 ( 0.2857142857142859205, 0.3035714285714287142, 0.3214285714285715634, 0.3392857142857143571, 0.3571428571428571508 ),
 .UNSPECIFIED. ) 
 CURVE ( )  GEOMETRIC_REPRESENTATION_ITEM ( )  RATIONAL_B_SPLINE_CURVE ( ( 0.9999999999999990008, 0.9238795325112877377, 1.000000000000000000, 0.9238795325112867385, 1.000000000000000000, 0.9238795325112867385, 1.000000000000000000, 0.9238795325112867385, 1.000000000000000000 ) ) 
 REPRESENTATION_ITEM ( '' )  );
#13618 = CARTESIAN_POINT ( 'NONE',  ( -2.066987300000001415, 64.85617417291294373, 47.90000000109247225 ) ) ;
#13619 = DIRECTION ( 'NONE',  ( -0.000000000000000000, 1.000000000000000000, -0.000000000000000000 ) ) ;
#13620 = ORIENTED_EDGE ( 'NONE', *, *, #5541, .F. ) ;
#13621 = CARTESIAN_POINT ( 'NONE',  ( -13.35725562635142794, -21.48433729119796709, 15.20117750791696132 ) ) ;
#13622 = PLANE ( 'NONE',  #6310 ) ;
#13623 = VERTEX_POINT ( 'NONE', #2875 ) ;
#13624 = CARTESIAN_POINT ( 'NONE',  ( 44.99999999999998579, -1.285879139104706187E-16, -53.39999999999999147 ) ) ;
#13625 = EDGE_LOOP ( 'NONE', ( #13903, #804, #17839, #15656 ) ) ;
#13626 = CARTESIAN_POINT ( 'NONE',  ( 3.099999999999998757, 0.000000000000000000, 1.500000000000000222 ) ) ;
#13627 = PRODUCT_DEFINITION ( 'UNKNOWN', '', #10149, #1397 ) ;
#13628 = LINE ( 'NONE', #1388, #4562 ) ;
#13629 = CIRCLE ( 'NONE', #14560, 6.000000000000003553 ) ;
#13630 = CARTESIAN_POINT ( 'NONE',  ( 0.000000000000000000, 64.00000000000000000, 49.99999999999999289 ) ) ;
#13631 = CONTEXT_DEPENDENT_SHAPE_REPRESENTATION ( #16459, #14421 ) ;
#13632 = AXIS2_PLACEMENT_3D ( 'NONE', #3205, #8013, #4789 ) ;
#13633 = FACE_OUTER_BOUND ( 'NONE', #14509, .T. ) ;
#13634 = DIRECTION ( 'NONE',  ( -0.000000000000000000, 1.000000000000000000, -0.000000000000000000 ) ) ;
#13635 = CARTESIAN_POINT ( 'NONE',  ( -19.24771351637089367, -21.35725562635142438, 40.13867750791695954 ) ) ;
#13636 = CARTESIAN_POINT ( 'NONE',  ( 0.000000000000000000, 64.00000000000000000, 49.99999999999999289 ) ) ;
#13637 = CARTESIAN_POINT ( 'NONE',  ( -9.955834737091912245, -22.82508104294696594, 21.10742750791695599 ) ) ;
#13638 = CARTESIAN_POINT ( 'NONE',  ( -37.50000000000002132, 0.000000000000000000, 24.99999999999998224 ) ) ;
#13639 = ORIENTED_EDGE ( 'NONE', *, *, #5061, .T. ) ;
#13640 = CARTESIAN_POINT ( 'NONE',  ( -19.99999999999999645, -24.16482700510261949, 15.42382249208304046 ) ) ;
#13641 = AXIS2_PLACEMENT_3D ( 'NONE', #2288, #13145, #3855 ) ;
#13642 = AXIS2_PLACEMENT_3D ( 'NONE', #18673, #9538, #5143 ) ;
#13643 = DIRECTION ( 'NONE',  ( -0.000000000000000000, 0.7071067811865456854, 0.7071067811865493491 ) ) ;
#13644 = CARTESIAN_POINT ( 'NONE',  ( -16.35725562635141372, -26.68048971390461332, 25.04882249208304401 ) ) ;
#13645 = CARTESIAN_POINT ( 'NONE',  ( -1.035533905932738641, 66.50000000000000000, 45.84999999999998721 ) ) ;
#13646 = VERTEX_POINT ( 'NONE', #14940 ) ;
#13647 = CARTESIAN_POINT ( 'NONE',  ( -10.15500167420339928, -22.00430890708279108, 4.586222366068608161E-17 ) ) ;
#13648 = ORIENTED_EDGE ( 'NONE', *, *, #10576, .T. ) ;
#13649 = CARTESIAN_POINT ( 'NONE',  ( -18.99999999999997513, 68.00000000000000000, 55.99999999999995026 ) ) ;
#13650 = CARTESIAN_POINT ( 'NONE',  ( 1.300000000000000044, 0.7390083445627193548, -1.280000000000000693 ) ) ;
#13651 = DIRECTION ( 'NONE',  ( -1.000000000000000000, 0.000000000000000000, 0.000000000000000000 ) ) ;
#13652 = DIRECTION ( 'NONE',  ( -0.9863224920830415687, -5.704848896154130918E-15, -0.1648270051026189120 ) ) ;
#13653 = VECTOR ( 'NONE', #1792, 1000.000000000000000 ) ;
#13654 = AXIS2_PLACEMENT_3D ( 'NONE', #13677, #1340, #256 ) ;
#13655 = LINE ( 'NONE', #4464, #18926 ) ;
#13656 = CARTESIAN_POINT ( 'NONE',  ( 4.189607678530260948, 26.72836399182260791, 59.40336399182267257 ) ) ;
#13657 = CARTESIAN_POINT ( 'NONE',  ( -24.00000000000000711, 53.00000000000000711, 20.00000000000000000 ) ) ;
#13658 = EDGE_LOOP ( 'NONE', ( #7848, #18378, #13414, #18831 ) ) ;
#13659 = ADVANCED_FACE ( 'NONE', ( #7479 ), #10608, .T. ) ;
#13660 = EDGE_CURVE ( 'NONE', #16697, #11555, #2965, .T. ) ;
#13661 = CARTESIAN_POINT ( 'NONE',  ( -32.50000000000000000, 58.00000000000000000, 15.00000000000000000 ) ) ;
#13662 = CARTESIAN_POINT ( 'NONE',  ( -11.46040770435012668, -27.78091578003887463, 11.48242750791695954 ) ) ;
#13663 = CARTESIAN_POINT ( 'NONE',  ( 1.767766952966369987, 65.76776695296638309, 48.20000000218494307 ) ) ;
#13664 = EDGE_CURVE ( 'NONE', #10761, #17265, #4552, .T. ) ;
#13665 = CARTESIAN_POINT ( 'NONE',  ( -12.35725562635140307, -28.24771351637085459, 18.92382249208304401 ) ) ;
#13666 = MECHANICAL_DESIGN_GEOMETRIC_PRESENTATION_REPRESENTATION (  '', ( #6795 ), #5542 ) ;
#13667 = CARTESIAN_POINT ( 'NONE',  ( -2.066987300000001415, 64.00000000000000000, 46.55000000109247082 ) ) ;
#13668 = CARTESIAN_POINT ( 'NONE',  ( -11.21908421996108629, -20.46040770435011069, 10.16992750791695244 ) ) ;
#13669 = EDGE_CURVE ( 'NONE', #201, #6864, #18629, .T. ) ;
#13670 = DIRECTION ( 'NONE',  ( -2.081668171172167774E-16, 0.000000000000000000, 1.000000000000000000 ) ) ;
#13671 = CARTESIAN_POINT ( 'NONE',  ( -12.35725562635143682, -19.75228648362908501, 15.20117750791695777 ) ) ;
#13672 = CARTESIAN_POINT ( 'NONE',  ( 7.500000000000005329, -26.00000000000000000, 12.50000000000000000 ) ) ;
#13673 = LINE ( 'NONE', #11731, #5708 ) ;
#13674 = CARTESIAN_POINT ( 'NONE',  ( 1.461580736456473684, 65.46158073645646880, 46.25000000109246656 ) ) ;
#13675 = CARTESIAN_POINT ( 'NONE',  ( -40.00000000000000711, 53.00000000000000711, 1.500000000000001332 ) ) ;
#13676 = DIRECTION ( 'NONE',  ( -0.000000000000000000, 1.000000000000000000, 1.632680918566406547E-16 ) ) ;
#13677 = CARTESIAN_POINT ( 'NONE',  ( -1.040834085586084257E-14, 29.74264068711926257, 56.74264068711929809 ) ) ;
#13678 = CARTESIAN_POINT ( 'NONE',  ( -2.066987300000001415, 64.00000000000000000, 46.55000000109247082 ) ) ;
#13679 = EDGE_CURVE ( 'NONE', #1168, #18345, #4458, .T. ) ;
#13680 = DIRECTION ( 'NONE',  ( -0.000000000000000000, -0.000000000000000000, -1.000000000000000000 ) ) ;
#13681 = COLOUR_RGB ( '', 0.31764706, 0.68627451, 0.89019608) ;
#13682 = FACE_OUTER_BOUND ( 'NONE', #14884, .T. ) ;
#13683 = VERTEX_POINT ( 'NONE', #5917 ) ;
#13684 = ORIENTED_EDGE ( 'NONE', *, *, #10439, .T. ) ;
#13685 = CARTESIAN_POINT ( 'NONE',  ( -18.35725562635138886, -30.14459132904237393, 19.79882249208303691 ) ) ;
#13686 = SURFACE_SIDE_STYLE ('',( #12317 ) ) ;
#13687 = CARTESIAN_POINT ( 'NONE',  ( -19.41254052147350961, -21.64274437364857562, 5.361322492083041347 ) ) ;
#13688 = ORIENTED_EDGE ( 'NONE', *, *, #7602, .F. ) ;
#13689 = EDGE_CURVE ( 'NONE', #12139, #428, #14838, .T. ) ;
#13690 = CARTESIAN_POINT ( 'NONE',  ( -12.68318583509884157, -21.92450931948787485, 10.16992750791695954 ) ) ;
#13691 = PLANE ( 'NONE',  #5812 ) ;
#13692 = CARTESIAN_POINT ( 'NONE',  ( -13.28918265808478694, -16.95583473709189093, 16.95507249208304046 ) ) ;
#13693 = CARTESIAN_POINT ( 'NONE',  ( 3.796994071234847710E-16, 61.93301269999999903, 45.75000000109247367 ) ) ;
#13694 = ORIENTED_EDGE ( 'NONE', *, *, #12853, .T. ) ;
#13695 = ORIENTED_EDGE ( 'NONE', *, *, #4751, .T. ) ;
#13696 = CARTESIAN_POINT ( 'NONE',  ( -7.499999999999994671, -38.00000000000000000, 4.500000000000000888 ) ) ;
#13697 = EDGE_LOOP ( 'NONE', ( #8130, #3626, #17241, #11370 ) ) ;
#13698 = EDGE_LOOP ( 'NONE', ( #13615, #6618, #18468, #12246 ) ) ;
#13699 = CARTESIAN_POINT ( 'NONE',  ( -2.066987300000001415, 64.85617417291294373, 48.70000000109247651 ) ) ;
#13700 = DIRECTION ( 'NONE',  ( 0.000000000000000000, 1.000000000000000000, 0.000000000000000000 ) ) ;
#13701 = CARTESIAN_POINT ( 'NONE',  ( -25.00000000000000000, 53.00000000000000711, 30.00000000000000000 ) ) ;
#13702 = EDGE_CURVE ( 'NONE', #6216, #2004, #1409, .T. ) ;
#13703 = EDGE_CURVE ( 'NONE', #18046, #14186, #17095, .T. ) ;
#13704 = APPLICATION_CONTEXT ( 'automotive_design' ) ;
#13705 = DIRECTION ( 'NONE',  ( -0.000000000000000000, -1.000000000000000000, -0.000000000000000000 ) ) ;
#13706 = EDGE_CURVE ( 'NONE', #11249, #13021, #3752, .T. ) ;
#13707 = DIRECTION ( 'NONE',  ( -0.000000000000000000, -1.000000000000000000, -0.000000000000000000 ) ) ;
#13708 = ORIENTED_EDGE ( 'NONE', *, *, #15989, .F. ) ;
#13710 = ORIENTED_EDGE ( 'NONE', *, *, #7719, .F. ) ;
#13709 = ORIENTED_EDGE ( 'NONE', *, *, #12480, .F. ) ;
#13711 = EDGE_CURVE ( 'NONE', #17737, #18430, #19006, .T. ) ;
#13712 = CARTESIAN_POINT ( 'NONE',  ( -18.35725562635144925, -17.85540867095761186, 19.57617750791695954 ) ) ;
#13713 = CARTESIAN_POINT ( 'NONE',  ( 0.000000000000000000, 0.000000000000000000, 0.000000000000000000 ) ) ;
#13714 = ORIENTED_EDGE ( 'NONE', *, *, #5814, .F. ) ;
#13715 = ORIENTED_EDGE ( 'NONE', *, *, #3155, .T. ) ;
#13716 = CARTESIAN_POINT ( 'NONE',  ( -12.31951028609536536, -25.35725562635139596, 13.23632249208304223 ) ) ;
#13717 = CARTESIAN_POINT ( 'NONE',  ( -21.99999999999999289, -23.83517299489739116, 8.201177507916955989 ) ) ;
#13718 = CARTESIAN_POINT ( 'NONE',  ( 1.461580736456473906, 62.53841926354353120, 49.05000000109247082 ) ) ;
#13719 = CARTESIAN_POINT ( 'NONE',  ( -32.50000000000000000, 47.00000000000000711, -35.00000000000000000 ) ) ;
#13720 = ORIENTED_EDGE ( 'NONE', *, *, #18946, .F. ) ;
#13721 = CARTESIAN_POINT ( 'NONE',  ( -17.68048971390461688, -25.35725562635141372, 13.01367750791696132 ) ) ;
#13722 = SURFACE_SIDE_STYLE ('',( #16975 ) ) ;
#13723 = ORIENTED_EDGE ( 'NONE', *, *, #1738, .T. ) ;
#13724 = CARTESIAN_POINT ( 'NONE',  ( -1.040834085586084257E-14, 29.74264068711926257, 56.74264068711929809 ) ) ;
#13725 = ORIENTED_EDGE ( 'NONE', *, *, #8897, .T. ) ;
#13726 = EDGE_CURVE ( 'NONE', #4727, #13491, #3371, .T. ) ;
#13727 = DIRECTION ( 'NONE',  ( -1.000000000000000000, -0.000000000000000000, -0.000000000000000000 ) ) ;
#13728 = LINE ( 'NONE', #591, #7157 ) ;
#13729 = FACE_BOUND ( 'NONE', #1728, .T. ) ;
#13730 = CARTESIAN_POINT ( 'NONE',  ( -41.00000000000000000, 47.00000000000000711, 18.00000000000000000 ) ) ;
#13731 = CARTESIAN_POINT ( 'NONE',  ( -40.00000000000000000, 53.00000000000000711, -50.00000000000000000 ) ) ;
#13732 = DIRECTION ( 'NONE',  ( -0.000000000000000000, 1.000000000000000000, -0.000000000000000000 ) ) ;
#13733 = VECTOR ( 'NONE', #16334, 1000.000000000000000 ) ;
#13734 = B_SPLINE_CURVE_WITH_KNOTS ( 'NONE', 3,
 ( #15742, #2304, #19059, #17591 ),
 .UNSPECIFIED., .F., .F.,
 ( 4, 4 ),
 ( 0.000000000000000000, 1.000000000000000000 ),
 .UNSPECIFIED. ) ;
#13735 = CARTESIAN_POINT ( 'NONE',  ( 11.00000000000000355, 0.000000000000000000, 0.000000000000000000 ) ) ;
#13736 = CARTESIAN_POINT ( 'NONE',  ( -43.50000000000000711, 118.0000000000000142, -52.50000000000000711 ) ) ;
#13737 = EDGE_LOOP ( 'NONE', ( #14304, #17954, #3408, #12714 ) ) ;
#13738 = CARTESIAN_POINT ( 'NONE',  ( -10.04416526290807710, -25.50457296725819489, 16.29492750791695954 ) ) ;
#13739 = CARTESIAN_POINT ( 'NONE',  ( -41.99999999999997868, 6.000000000000005329, -52.00000000000000000 ) ) ;
#13740 = ORIENTED_EDGE ( 'NONE', *, *, #12480, .T. ) ;
#13741 = CARTESIAN_POINT ( 'NONE',  ( -20.04416526290809131, -22.82508104294699791, 20.89257249208303691 ) ) ;
#13742 = PRODUCT_RELATED_PRODUCT_CATEGORY ( 'part', '', ( #12846 ) ) ;
#13743 = TOROIDAL_SURFACE ( 'NONE', #3417, 1.600000000000000311, 0.1000000000000000056 ) ;
#13744 = CARTESIAN_POINT ( 'NONE',  ( -14.03132541760400009, -26.95583473709189448, 19.14257249208304401 ) ) ;
#13745 = AXIS2_PLACEMENT_3D ( 'NONE', #16924, #9356, #7802 ) ;
#13746 = DIRECTION ( 'NONE',  ( -1.000000000000000000, 0.000000000000000000, 0.000000000000000000 ) ) ;
#13747 = ORIENTED_EDGE ( 'NONE', *, *, #6126, .F. ) ;
#13748 = FACE_OUTER_BOUND ( 'NONE', #13020, .T. ) ;
#13749 = VERTEX_POINT ( 'NONE', #4847 ) ;
#13750 = ADVANCED_FACE ( 'NONE', ( #5141 ), #12983, .F. ) ;
#13751 = DIRECTION ( 'NONE',  ( 7.602811950582247805E-15, 0.000000000000000000, -1.000000000000000000 ) ) ;
#13752 = CARTESIAN_POINT ( 'NONE',  ( -41.00000000000000711, 53.00000000000000711, -12.50000000000000000 ) ) ;
#13753 = CARTESIAN_POINT ( 'NONE',  ( 3.099999999999998757, 1.959434878635765477E-16, 1.600000000000000311 ) ) ;
#13754 = FACE_BOUND ( 'NONE', #561, .T. ) ;
#13755 = CIRCLE ( 'NONE', #917, 2.500000000000001776 ) ;
#13756 = LINE ( 'NONE', #1094, #11698 ) ;
#13757 = FACE_OUTER_BOUND ( 'NONE', #13233, .T. ) ;
#13758 = FACE_OUTER_BOUND ( 'NONE', #2457, .T. ) ;
#13759 = CIRCLE ( 'NONE', #12804, 0.2500000000000002220 ) ;
#13760 = VECTOR ( 'NONE', #6071, 1000.000000000000000 ) ;
#13761 = UNCERTAINTY_MEASURE_WITH_UNIT (LENGTH_MEASURE( 1.000000000000000082E-05 ), #7858, 'distance_accuracy_value', 'NONE');
#13762 = ORIENTED_EDGE ( 'NONE', *, *, #11381, .F. ) ;
#13763 = DIRECTION ( 'NONE',  ( 0.000000000000000000, 1.000000000000000000, 0.000000000000000000 ) ) ;
#13764 = CARTESIAN_POINT ( 'NONE',  ( -17.64274437364855430, -28.24771351637087236, 17.82617750791695599 ) ) ;
#13765 = AXIS2_PLACEMENT_3D ( 'NONE', #6192, #17750, #9016 ) ;
#13766 = CARTESIAN_POINT ( 'NONE',  ( 2.500000000000001776, 65.03553390593273775, 44.95000000218494307 ) ) ;
#13767 = CARTESIAN_POINT ( 'NONE',  ( -19.95583473709190514, -25.50457296725822687, 20.45507249208304401 ) ) ;
#13768 = VECTOR ( 'NONE', #8357, 1000.000000000000000 ) ;
#13769 = PLANE ( 'NONE',  #12283 ) ;
#13770 = CARTESIAN_POINT ( 'NONE',  ( -16.50457296725820555, -28.95583473709189448, 22.85742750791695954 ) ) ;
#13771 = LINE ( 'NONE', #16060, #6102 ) ;
#13772 = CARTESIAN_POINT ( 'NONE',  ( -19.99999999999999645, -23.83517299489738051, 18.70117750791695954 ) ) ;
#13773 = VECTOR ( 'NONE', #12549, 1000.000000000000000 ) ;
#13774 = DIRECTION ( 'NONE',  ( 0.000000000000000000, 0.000000000000000000, -1.000000000000000000 ) ) ;
#13775 = DIRECTION ( 'NONE',  ( -0.000000000000000000, -1.000000000000000000, -0.000000000000000000 ) ) ;
#13776 = CARTESIAN_POINT ( 'NONE',  ( 2.066987300000001415, 64.00000000000000000, 48.55000000109247082 ) ) ;
#13777 = DIRECTION ( 'NONE',  ( 0.000000000000000000, -0.000000000000000000, 1.000000000000000000 ) ) ;
#13778 = CARTESIAN_POINT ( 'NONE',  ( -41.00000000000000711, 110.0000000000000000, 6.999999999999999112 ) ) ;
#13779 = VECTOR ( 'NONE', #14232, 1000.000000000000000 ) ;
#13780 = DIRECTION ( 'NONE',  ( -0.000000000000000000, -0.000000000000000000, -1.000000000000000000 ) ) ;
#13781 = CARTESIAN_POINT ( 'NONE',  ( -1.461580736456473906, 65.46158073645646880, 47.25000000109246656 ) ) ;
#13782 = LINE ( 'NONE', #9080, #9865 ) ;
#13783 = ORIENTED_EDGE ( 'NONE', *, *, #13258, .F. ) ;
#13784 = ORIENTED_EDGE ( 'NONE', *, *, #5181, .T. ) ;
#13785 = CARTESIAN_POINT ( 'NONE',  ( -7.999999999999996447, -23.83517299489733432, 33.79882249208304046 ) ) ;
#13786 =( NAMED_UNIT ( * ) SI_UNIT ( $, .STERADIAN. ) SOLID_ANGLE_UNIT ( ) );
#13787 = CARTESIAN_POINT ( 'NONE',  ( -19.24771351637086880, -26.64274437364857206, 9.736322492083042235 ) ) ;
#13788 = ORIENTED_EDGE ( 'NONE', *, *, #8811, .T. ) ;
#13789 = CARTESIAN_POINT ( 'NONE',  ( -13.35725562635142794, -21.48433729119796709, 36.20117750791695954 ) ) ;
#13790 = CARTESIAN_POINT ( 'NONE',  ( 0.000000000000000000, -1.178949249685214307, 2.042000000000002036 ) ) ;
#13791 = CARTESIAN_POINT ( 'NONE',  ( -8.044165262908093084, -21.95952864787946979, 23.08007249208303691 ) ) ;
#13792 = VECTOR ( 'NONE', #3819, 1000.000000000000114 ) ;
#13793 = CARTESIAN_POINT ( 'NONE',  ( -3.400000000000017675, 29.83102903476760659, 56.65425233947095762 ) ) ;
#13794 = CARTESIAN_POINT ( 'NONE',  ( -1.461580736456473462, 62.53841926354353120, 48.05000000109247082 ) ) ;
#13795 = EDGE_LOOP ( 'NONE', ( #482, #14381, #6724, #19346 ) ) ;
#13796 = ORIENTED_EDGE ( 'NONE', *, *, #8565, .T. ) ;
#13797 = PLANE ( 'NONE',  #4428 ) ;
#13798 = FACE_OUTER_BOUND ( 'NONE', #16347, .T. ) ;
#13799 = AXIS2_PLACEMENT_3D ( 'NONE', #17560, #17957, #4529 ) ;
#13800 = ORIENTED_EDGE ( 'NONE', *, *, #11039, .F. ) ;
#13801 = CARTESIAN_POINT ( 'NONE',  ( 3.000000000000002665, 0.000000000000000000, 0.000000000000000000 ) ) ;
#13802 = CARTESIAN_POINT ( 'NONE',  ( -31.74999999999995737, 0.000000000000000000, 2.500000000000000444 ) ) ;
#13803 = EDGE_CURVE ( 'NONE', #6518, #17050, #12667, .T. ) ;
#13804 = AXIS2_PLACEMENT_3D ( 'NONE', #6560, #3609, #11142 ) ;
#13805 = DIRECTION ( 'NONE',  ( 2.775557561562891844E-16, 0.7071067811865453523, 0.7071067811865497932 ) ) ;
#13806 = FACE_OUTER_BOUND ( 'NONE', #13795, .T. ) ;
#13807 = CARTESIAN_POINT ( 'NONE',  ( -2.500000000000001776, 64.00000000000000000, 45.30000000218493739 ) ) ;
#13808 = ORIENTED_EDGE ( 'NONE', *, *, #10931, .F. ) ;
#13810 = ORIENTED_EDGE ( 'NONE', *, *, #12249, .F. ) ;
#13809 = ORIENTED_EDGE ( 'NONE', *, *, #17416, .T. ) ;
#13811 = CARTESIAN_POINT ( 'NONE',  ( -14.83517299489740715, -16.99999999999997868, 25.26367750791695954 ) ) ;
#13812 = CARTESIAN_POINT ( 'NONE',  ( 2.500000000000001776, 64.00000000000000000, 49.60000000000000142 ) ) ;
#13813 = VECTOR ( 'NONE', #2164, 1000.000000000000114 ) ;
#13814 = VERTEX_POINT ( 'NONE', #11097 ) ;
#13816 = ORIENTED_EDGE ( 'NONE', *, *, #13342, .F. ) ;
#13815 = ORIENTED_EDGE ( 'NONE', *, *, #1150, .F. ) ;
#13817 = CARTESIAN_POINT ( 'NONE',  ( -17.51566270880199738, -25.64274437364856496, 20.23632249208304401 ) ) ;
#13818 = CARTESIAN_POINT ( 'NONE',  ( -21.14459132904236327, -27.35725562635143149, 23.51367750791695599 ) ) ;
#13819 = EDGE_CURVE ( 'NONE', #17611, #4643, #18473, .T. ) ;
#13820 = ADVANCED_FACE ( 'NONE', ( #3467, #4949 ), #11188, .F. ) ;
#13821 = CARTESIAN_POINT ( 'NONE',  ( -1.461580736456473906, 65.46158073645646880, 48.65000000109247225 ) ) ;
#13822 = DIRECTION ( 'NONE',  ( 0.000000000000000000, 0.000000000000000000, -1.000000000000000000 ) ) ;
#13823 = ORIENTED_EDGE ( 'NONE', *, *, #11284, .T. ) ;
#13824 = ADVANCED_FACE ( 'NONE', ( #11003 ), #9533, .F. ) ;
#13825 = CARTESIAN_POINT ( 'NONE',  ( -11.95583473709191047, -23.36097942780921954, 15.85742750791696309 ) ) ;
#13826 = VECTOR ( 'NONE', #8489, 1000.000000000000000 ) ;
#13827 = EDGE_LOOP ( 'NONE', ( #3068, #16968, #18624, #11340, #3364, #7584, #4288 ) ) ;
#13828 = DIRECTION ( 'NONE',  ( 1.000000000000000000, 0.000000000000000000, -7.709882115452476934E-17 ) ) ;
#13829 = EDGE_LOOP ( 'NONE', ( #9230, #11424, #16656, #2527 ) ) ;
#13830 = DIRECTION ( 'NONE',  ( -0.000000000000000000, -0.000000000000000000, -1.000000000000000000 ) ) ;
#13831 = DIRECTION ( 'NONE',  ( 0.000000000000000000, 1.000000000000000000, 0.000000000000000000 ) ) ;
#13832 = CARTESIAN_POINT ( 'NONE',  ( -25.00000000000000711, 110.0000000000000000, 26.50000000000000000 ) ) ;
#13833 = PLANE ( 'NONE',  #15817 ) ;
#13834 = DIRECTION ( 'NONE',  ( -0.000000000000000000, -0.000000000000000000, -1.000000000000000000 ) ) ;
#13835 = AXIS2_PLACEMENT_3D ( 'NONE', #15063, #2901, #4184 ) ;
#13836 = ITEM_DEFINED_TRANSFORMATION ( 'NONE', 'NONE', #6111,  #1791 ) ;
#13837 = CARTESIAN_POINT ( 'NONE',  ( -1.530808498934192803E-16, 66.50000000000000000, 49.10000000218494165 ) ) ;
#13838 = LINE ( 'NONE', #506, #16288 ) ;
#13839 = VECTOR ( 'NONE', #14677, 1000.000000000000000 ) ;
#13840 = CARTESIAN_POINT ( 'NONE',  ( 0.000000000000000000, 64.00000000000000000, 49.99999999999999289 ) ) ;
#13841 = LINE ( 'NONE', #18457, #4887 ) ;
#13842 = ORIENTED_EDGE ( 'NONE', *, *, #16957, .F. ) ;
#13843 = CARTESIAN_POINT ( 'NONE',  ( -14.83517299489739649, -18.99999999999997868, 20.01367750791695954 ) ) ;
#13844 = DIRECTION ( 'NONE',  ( 1.000000000000000000, -0.000000000000000000, -0.000000000000000000 ) ) ;
#13845 = ORIENTED_EDGE ( 'NONE', *, *, #957, .T. ) ;
#13846 = CARTESIAN_POINT ( 'NONE',  ( -10.58745947852648328, -26.35725562635138530, 18.48632249208304401 ) ) ;
#13847 = ADVANCED_FACE ( 'NONE', ( #9723 ), #15718, .F. ) ;
#13848 = CARTESIAN_POINT ( 'NONE',  ( -11.99999999999999289, -23.83517299489735564, 12.79882249208304223 ) ) ;
#13849 = AXIS2_PLACEMENT_3D ( 'NONE', #10822, #12592, #12395 ) ;
#13850 = PLANE ( 'NONE',  #8170 ) ;
#13851 = ORIENTED_EDGE ( 'NONE', *, *, #9280, .F. ) ;
#13852 = LINE ( 'NONE', #7980, #6255 ) ;
#13853 = ORIENTED_EDGE ( 'NONE', *, *, #5654, .F. ) ;
#13854 = CARTESIAN_POINT ( 'NONE',  ( -5.800000000000006928, 29.47747564417435484, 56.65425233947093631 ) ) ;
#13855 = CARTESIAN_POINT ( 'NONE',  ( 2.500000000000007105, 62.96446609406726225, 46.34999999999998721 ) ) ;
#13856 = CARTESIAN_POINT ( 'NONE',  ( -44.99999999999998579, 3.000000000000000000, -53.50000000000000000 ) ) ;
#13857 = VECTOR ( 'NONE', #15376, 1000.000000000000000 ) ;
#13858 = DIRECTION ( 'NONE',  ( 1.000000000000000000, 0.000000000000000000, 0.000000000000000000 ) ) ;
#13859 = DIRECTION ( 'NONE',  ( 1.000000000000000000, -0.000000000000000000, -0.000000000000000000 ) ) ;
#13860 = FILL_AREA_STYLE ('',( #10909 ) ) ;
#13861 = DIRECTION ( 'NONE',  ( -1.000000000000000000, 0.000000000000000000, -0.000000000000000000 ) ) ;
#13862 = ADVANCED_FACE ( 'NONE', ( #2184 ), #9442, .T. ) ;
#13863 = ORIENTED_EDGE ( 'NONE', *, *, #2398, .F. ) ;
#13864 = DIRECTION ( 'NONE',  ( 1.000000000000000000, 0.000000000000000000, 0.000000000000000000 ) ) ;
#13865 = CARTESIAN_POINT ( 'NONE',  ( -10.75228648362910100, -26.64274437364854009, 16.51367750791695954 ) ) ;
#13866 = CARTESIAN_POINT ( 'NONE',  ( -1.035533905932738863, 61.50000000000000000, 47.05000000218494449 ) ) ;
#13867 = CARTESIAN_POINT ( 'NONE',  ( -12.64274437364858628, -19.58745947852646552, 17.17382249208304401 ) ) ;
#13868 = CARTESIAN_POINT ( 'NONE',  ( 44.99999999999997158, -1.285879139104706187E-16, 55.00000000000000000 ) ) ;
#13869 = EDGE_CURVE ( 'NONE', #13949, #14586, #7784, .T. ) ;
#13870 = CARTESIAN_POINT ( 'NONE',  ( -19.99999999999999645, -23.83517299489738051, 13.45117750791695777 ) ) ;
#13871 = DIRECTION ( 'NONE',  ( 0.000000000000000000, -1.000000000000000000, 0.000000000000000000 ) ) ;
#13872 = CARTESIAN_POINT ( 'NONE',  ( -10.75228648362910100, -26.64274437364854009, 21.76367750791695599 ) ) ;
#13873 = DIRECTION ( 'NONE',  ( 1.000000000000000000, -0.000000000000000000, 0.000000000000000000 ) ) ;
#13874 = FACE_BOUND ( 'NONE', #13400, .T. ) ;
#13875 = CARTESIAN_POINT ( 'NONE',  ( 2.066987300000001859, 64.85617417291294373, 47.00000000109246656 ) ) ;
#13876 = CARTESIAN_POINT ( 'NONE',  ( -24.00000000000000000, 53.00000000000000711, 30.00000000000000000 ) ) ;
#13877 = CARTESIAN_POINT ( 'NONE',  ( 0.000000000000000000, 3.275930187719169848E-16, -2.600000000000000089 ) ) ;
#13878 = PRESENTATION_STYLE_ASSIGNMENT (( #12407 ) ) ;
#13879 = CARTESIAN_POINT ( 'NONE',  ( 2.066987300000002303, 63.14382582708705627, 48.50000000109246656 ) ) ;
#13880 = DIRECTION ( 'NONE',  ( 1.000000000000000000, -0.000000000000000000, -0.000000000000000000 ) ) ;
#13882 = ORIENTED_EDGE ( 'NONE', *, *, #7566, .T. ) ;
#13881 = ADVANCED_FACE ( 'NONE', ( #18280 ), #10806, .T. ) ;
#13883 = EDGE_LOOP ( 'NONE', ( #13087, #7582, #14936, #9899 ) ) ;
#13884 = CARTESIAN_POINT ( 'NONE',  ( -13.28918265808478694, -16.95583473709189093, 27.45507249208304046 ) ) ;
#13885 = CARTESIAN_POINT ( 'NONE',  ( -17.64274437364858983, -19.75228648362910633, 11.04882249208304046 ) ) ;
#13886 = ORIENTED_EDGE ( 'NONE', *, *, #10675, .F. ) ;
#13887 = CARTESIAN_POINT ( 'NONE',  ( -14.83517299489738761, -20.99999999999997513, 30.51367750791696309 ) ) ;
#13888 = LINE ( 'NONE', #11356, #12994 ) ;
#13889 = CARTESIAN_POINT ( 'NONE',  ( -22.04416526290809486, -22.28918265808477628, 20.89257249208303691 ) ) ;
#13890 = CARTESIAN_POINT ( 'NONE',  ( 0.8561741729129460632, 66.06698729999999387, 46.10000000109246798 ) ) ;
#13891 = CARTESIAN_POINT ( 'NONE',  ( -1.461580736456473906, 65.46158073645646880, 45.45000000109246940 ) ) ;
#13892 = ORIENTED_EDGE ( 'NONE', *, *, #1384, .T. ) ;
#13893 = EDGE_LOOP ( 'NONE', ( #5490, #3140, #3235, #16374 ) ) ;
#13894 = DIRECTION ( 'NONE',  ( -0.7071067811865437980, 0.5000000000000043299, -0.5000000000000008882 ) ) ;
#13895 = DIRECTION ( 'NONE',  ( -1.156482317317871478E-16, 1.000000000000000000, 0.000000000000000000 ) ) ;
#13896 = CARTESIAN_POINT ( 'NONE',  ( 2.749999999999979128, 118.0000000000000142, 37.49999999999997158 ) ) ;
#13897 = LINE ( 'NONE', #12618, #9682 ) ;
#13898 = CARTESIAN_POINT ( 'NONE',  ( -24.00000000000000000, 110.0000000000000000, -38.50000000000000711 ) ) ;
#13899 = VECTOR ( 'NONE', #16019, 1000.000000000000000 ) ;
#13900 = CARTESIAN_POINT ( 'NONE',  ( -3.065533689247737392, -46.96461745799954457, 3.000000000000000000 ) ) ;
#13901 = CARTESIAN_POINT ( 'NONE',  ( -1.035533905932738641, 66.50000000000000000, 47.55000000218494449 ) ) ;
#13902 = VERTEX_POINT ( 'NONE', #430 ) ;
#13904 = ORIENTED_EDGE ( 'NONE', *, *, #7448, .T. ) ;
#13903 = ORIENTED_EDGE ( 'NONE', *, *, #15975, .F. ) ;
#13905 = CARTESIAN_POINT ( 'NONE',  ( -20.00369391078762860, -18.75498260482333279, 35.10742750791695244 ) ) ;
#13906 = SHAPE_REPRESENTATION ( 'Removable Bottom Crumb Tray', ( #1791 ), #5851 ) ;
#13907 = ORIENTED_EDGE ( 'NONE', *, *, #2678, .T. ) ;
#13908 = ORIENTED_EDGE ( 'NONE', *, *, #13110, .F. ) ;
#13909 = CARTESIAN_POINT ( 'NONE',  ( -17.99999999999999645, -24.16482700510260173, 36.42382249208304756 ) ) ;
#13910 = EDGE_CURVE ( 'NONE', #7059, #13385, #12381, .T. ) ;
#13911 = EDGE_CURVE ( 'NONE', #5613, #1200, #12758, .T. ) ;
#13912 = CARTESIAN_POINT ( 'NONE',  ( -7.999999999999996447, -24.16482700510256976, 21.32617750791695599 ) ) ;
#13913 = CARTESIAN_POINT ( 'NONE',  ( 2.066987300000001859, 63.14382582708704916, 49.10000000109246088 ) ) ;
#13914 = DIRECTION ( 'NONE',  ( 1.000000000000000000, 0.000000000000000000, 2.973811673103096679E-16 ) ) ;
#13915 = ORIENTED_EDGE ( 'NONE', *, *, #384, .F. ) ;
#13916 = CARTESIAN_POINT ( 'NONE',  ( -12.48433729119798130, -25.64274437364855075, 16.51367750791695954 ) ) ;
#13917 = EDGE_CURVE ( 'NONE', #2170, #5957, #17366, .T. ) ;
#13918 = LINE ( 'NONE', #12258, #10663 ) ;
#13919 = ORIENTED_EDGE ( 'NONE', *, *, #1576, .T. ) ;
#13920 = CARTESIAN_POINT ( 'NONE',  ( -50.00000000000002132, 33.00000000000000000, 40.49999999999996447 ) ) ;
#13921 = ORIENTED_EDGE ( 'NONE', *, *, #744, .F. ) ;
#13922 = CARTESIAN_POINT ( 'NONE',  ( -25.00000000000000711, 110.0000000000000000, -32.00000000000000000 ) ) ;
#13923 = DIRECTION ( 'NONE',  ( -1.734723475976807094E-15, 1.000000000000000000, 0.000000000000000000 ) ) ;
#13924 = FACE_OUTER_BOUND ( 'NONE', #2622, .T. ) ;
#13925 = DIRECTION ( 'NONE',  ( 0.000000000000000000, -0.000000000000000000, 1.000000000000000000 ) ) ;
#13926 = EDGE_CURVE ( 'NONE', #4628, #6193, #17561, .T. ) ;
#13927 = CARTESIAN_POINT ( 'NONE',  ( -41.00000000000000711, 110.0000000000000000, 21.00000000000000000 ) ) ;
#13928 = CARTESIAN_POINT ( 'NONE',  ( 3.796994071234847710E-16, 61.93301269999999903, 48.15000000109247225 ) ) ;
#13929 = CONTEXT_DEPENDENT_SHAPE_REPRESENTATION ( #17833, #3009 ) ;
#13930 = LINE ( 'NONE', #6098, #14929 ) ;
#13931 = DIRECTION ( 'NONE',  ( 0.000000000000000000, -1.000000000000000000, 1.287488025362403787E-15 ) ) ;
#13932 = AXIS2_PLACEMENT_3D ( 'NONE', #1626, #9254, #15241 ) ;
#13933 = DIRECTION ( 'NONE',  ( 0.000000000000000000, 0.000000000000000000, 1.000000000000000000 ) ) ;
#13934 = VECTOR ( 'NONE', #17883, 1000.000000000000000 ) ;
#13935 = DIRECTION ( 'NONE',  ( 0.000000000000000000, -0.4999999999999991118, 0.8660254037844390407 ) ) ;
#13936 = ORIENTED_EDGE ( 'NONE', *, *, #15140, .F. ) ;
#13937 = EDGE_CURVE ( 'NONE', #5315, #587, #6974, .T. ) ;
#13938 = CARTESIAN_POINT ( 'NONE',  ( -16.17491895705301275, -18.95583473709189803, 25.04492750791695954 ) ) ;
#13939 = FACE_OUTER_BOUND ( 'NONE', #11186, .T. ) ;
#13940 = ORIENTED_EDGE ( 'NONE', *, *, #6802, .T. ) ;
#13941 = CARTESIAN_POINT ( 'NONE',  ( -17.35725562635140307, -28.41254052147349185, 35.54882249208304046 ) ) ;
#13942 = EDGE_CURVE ( 'NONE', #15953, #5501, #8449, .T. ) ;
#13943 = CARTESIAN_POINT ( 'NONE',  ( -17.99999999999999645, -24.16482700510260173, 20.67382249208304046 ) ) ;
#13944 = LINE ( 'NONE', #519, #11897 ) ;
#13945 = EDGE_LOOP ( 'NONE', ( #9035, #577, #2491, #18997 ) ) ;
#13946 = B_SPLINE_CURVE_WITH_KNOTS ( 'NONE', 3,
 ( #10789, #6400, #8068, #12563, #5129, #9976, #12652, #5402, #14222, #11171, #3920, #2443, #14131, #8427, #18652, #980, #15979, #8524 ),
 .UNSPECIFIED., .F., .F.,
 ( 4, 2, 2, 2, 2, 2, 2, 2, 4 ),
 ( 0.000000000000000000, 0.0005599264810181958478, 0.001119852962036391696, 0.001679779443054587543, 0.002239705924072783391, 0.002799632405090979239, 0.003359558886109175087, 0.003919485367127341011, 0.004479411848145506067 ),
 .UNSPECIFIED. ) ;
#13947 = VECTOR ( 'NONE', #409, 1000.000000000000000 ) ;
#13948 = DIRECTION ( 'NONE',  ( 0.000000000000000000, 0.000000000000000000, -1.000000000000000000 ) ) ;
#13949 = VERTEX_POINT ( 'NONE', #16086 ) ;
#13950 = FACE_OUTER_BOUND ( 'NONE', #14196, .T. ) ;
#13951 = DIRECTION ( 'NONE',  ( -0.000000000000000000, -0.000000000000000000, -1.000000000000000000 ) ) ;
#13952 = DIRECTION ( 'NONE',  ( -1.000000000000000000, 0.000000000000000000, 0.000000000000000000 ) ) ;
#13953 = CARTESIAN_POINT ( 'NONE',  ( 4.189607678530260948, 26.72836399182260791, 59.40336399182267257 ) ) ;
#13954 = ADVANCED_FACE ( 'NONE', ( #807 ), #15898, .T. ) ;
#13955 = ADVANCED_FACE ( 'NONE', ( #12941 ), #11281, .T. ) ;
#13956 = CARTESIAN_POINT ( 'NONE',  ( -24.00000000000000711, 53.00000000000000711, -32.00000000000000000 ) ) ;
#13957 = DIRECTION ( 'NONE',  ( 0.000000000000000000, -1.000000000000000000, -0.000000000000000000 ) ) ;
#13958 = VECTOR ( 'NONE', #19209, 1000.000000000000000 ) ;
#13959 = VECTOR ( 'NONE', #5685, 1000.000000000000000 ) ;
#13960 = EDGE_LOOP ( 'NONE', ( #4528, #9203, #16277, #15479, #18992, #15884, #12224, #6678, #2919, #15755, #9047, #11520, #4813, #6816, #9948, #12844, #12550, #6606, #2132, #9148, #18069, #15956, #18863, #13008, #11412, #15862, #12913, #8500, #10773, #1659, #13788, #7422, #17068, #8134, #4712, #10227, #7040, #4795, #18633, #2449, #14475, #10993, #19301, #17547, #7417, #11627, #13892, #8980, #10484, #5475, #12325, #8607 ) ) ;
#13961 = EDGE_CURVE ( 'NONE', #12028, #19093, #18937, .T. ) ;
#13962 = CARTESIAN_POINT ( 'NONE',  ( -12.35725562635143682, -19.75228648362908501, 20.45117750791695954 ) ) ;
#13963 = CARTESIAN_POINT ( 'NONE',  ( -1.035533905932738641, 66.50000000000000000, 45.15000000218493881 ) ) ;
#13964 = CARTESIAN_POINT ( 'NONE',  ( -13.49542703274174116, -28.95583473709188738, 13.89257249208303691 ) ) ;
#13965 = CARTESIAN_POINT ( 'NONE',  ( -25.00000000000000000, 53.00000000000000711, -38.50000000000000711 ) ) ;
#13966 = CARTESIAN_POINT ( 'NONE',  ( -9.999999999999994671, -24.16482700510257686, 16.07617750791695954 ) ) ;
#13967 = CYLINDRICAL_SURFACE ( 'NONE', #15808, 2.500000000000001776 ) ;
#13968 = CIRCLE ( 'NONE', #8627, 2.500000000000001776 ) ;
#13969 = CARTESIAN_POINT ( 'NONE',  ( -13.49542703274178201, -19.04416526290806289, 14.98242750791695777 ) ) ;
#13970 = DIRECTION ( 'NONE',  ( -0.000000000000000000, 1.000000000000000000, -0.000000000000000000 ) ) ;
#13971 = CARTESIAN_POINT ( 'NONE',  ( -9.999999999999994671, -23.83517299489734143, 23.29882249208304046 ) ) ;
#13972 = AXIS2_PLACEMENT_3D ( 'NONE', #16119, #13366, #4266 ) ;
#13973 = EDGE_CURVE ( 'NONE', #89, #16741, #5505, .T. ) ;
#13974 = CARTESIAN_POINT ( 'NONE',  ( 2.066987300000001859, 64.85617417291294373, 48.60000000109246798 ) ) ;
#13975 = DIRECTION ( 'NONE',  ( 1.000000000000000000, 0.000000000000000000, 0.000000000000000000 ) ) ;
#13976 = CARTESIAN_POINT ( 'NONE',  ( -41.00000000000000711, 53.00000000000000711, -11.50000000000000000 ) ) ;
#13977 = CARTESIAN_POINT ( 'NONE',  ( 2.500000000000001776, 64.00000000000000000, 49.99999999999999289 ) ) ;
#13978 = CARTESIAN_POINT ( 'NONE',  ( -2.066987300000001859, 64.85617417291294373, 48.90000000109247225 ) ) ;
#13979 = CARTESIAN_POINT ( 'NONE',  ( -18.99999999999997513, 60.00000000000000711, 55.99999999999995026 ) ) ;
#13980 = ORIENTED_EDGE ( 'NONE', *, *, #11228, .F. ) ;
#13981 = ORIENTED_EDGE ( 'NONE', *, *, #7485, .T. ) ;
#13982 = CARTESIAN_POINT ( 'NONE',  ( -17.04047135212050890, -17.04416526290807710, 27.01757249208303691 ) ) ;
#13983 = VECTOR ( 'NONE', #6689, 999.9999999999998863 ) ;
#13984 = AXIS2_PLACEMENT_3D ( 'NONE', #15217, #9132, #10691 ) ;
#13985 = CARTESIAN_POINT ( 'NONE',  ( -20.04416526290809131, -22.82508104294700502, 15.64257249208304223 ) ) ;
#13986 = VERTEX_POINT ( 'NONE', #11468 ) ;
#13987 = CARTESIAN_POINT ( 'NONE',  ( -15.96867458239597326, -26.95583473709190159, 28.10742750791695954 ) ) ;
#13988 = CARTESIAN_POINT ( 'NONE',  ( 32.49999999999998579, 0.000000000000000000, 42.49999999999997868 ) ) ;
#13989 = CARTESIAN_POINT ( 'NONE',  ( -20.00369391078757886, -29.24501739517668142, 25.26757249208304401 ) ) ;
#13990 = CARTESIAN_POINT ( 'NONE',  ( -1.265664690411616068E-16, 66.06698730000000808, 46.95000000109246940 ) ) ;
#13991 = FACE_OUTER_BOUND ( 'NONE', #18435, .T. ) ;
#13992 = VERTEX_POINT ( 'NONE', #3848 ) ;
#13993 = EDGE_LOOP ( 'NONE', ( #10145, #19288 ) ) ;
#13994 = LINE ( 'NONE', #12228, #15665 ) ;
#13995 = CARTESIAN_POINT ( 'NONE',  ( -15.20357423236093375, -43.78611686177728046, 3.000000000000000000 ) ) ;
#13996 = CARTESIAN_POINT ( 'NONE',  ( 0.8561741729129460632, 66.06698730000000808, 48.50000000109246656 ) ) ;
#13997 = CARTESIAN_POINT ( 'NONE',  ( 24.00000000000000000, -0.000000000000000000, 18.00000000000000000 ) ) ;
#13998 = CARTESIAN_POINT ( 'NONE',  ( -1.265664690411616068E-16, 66.06698730000000808, 44.75000000109247367 ) ) ;
#13999 = FACE_OUTER_BOUND ( 'NONE', #15893, .T. ) ;
#14000 = CARTESIAN_POINT ( 'NONE',  ( -21.50000000000000000, 118.0000000000000142, 32.50000000000000000 ) ) ;
#14001 = ORIENTED_EDGE ( 'NONE', *, *, #13819, .F. ) ;
#14002 = ORIENTED_EDGE ( 'NONE', *, *, #16388, .T. ) ;
#14003 = CARTESIAN_POINT ( 'NONE',  ( -9.754982604823348780, -18.99630608921234654, 25.91992750791695599 ) ) ;
#14004 = FILL_AREA_STYLE ('',( #12143 ) ) ;
#14005 = VERTEX_POINT ( 'NONE', #17656 ) ;
#14007 = ORIENTED_EDGE ( 'NONE', *, *, #16721, .T. ) ;
#14006 = ORIENTED_EDGE ( 'NONE', *, *, #16089, .T. ) ;
#14008 = CARTESIAN_POINT ( 'NONE',  ( -15.96867458239599635, -21.04416526290806999, 37.51757249208305467 ) ) ;
#14009 = CARTESIAN_POINT ( 'NONE',  ( -16.71081734191527346, -16.95583473709190159, 14.54492750791695421 ) ) ;
#14010 = DIRECTION ( 'NONE',  ( 0.000000000000000000, -1.000000000000000000, 0.000000000000000000 ) ) ;
#14011 = CARTESIAN_POINT ( 'NONE',  ( 7.500000000000005329, -26.00000000000000000, 1.500000000000000000 ) ) ;
#14012 = CYLINDRICAL_SURFACE ( 'NONE', #318, 2.999999999999999112 ) ;
#14013 = ORIENTED_EDGE ( 'NONE', *, *, #8398, .T. ) ;
#14014 = CARTESIAN_POINT ( 'NONE',  ( -12.68318583509884157, -21.92450931948787485, 25.91992750791696309 ) ) ;
#14015 = CARTESIAN_POINT ( 'NONE',  ( 2.500000000000000000, -1.178949249685214307, 2.042000000000002036 ) ) ;
#14016 = ORIENTED_EDGE ( 'NONE', *, *, #8755, .T. ) ;
#14017 = DIRECTION ( 'NONE',  ( 0.000000000000000000, 0.000000000000000000, 1.000000000000000000 ) ) ;
#14018 = ORIENTED_EDGE ( 'NONE', *, *, #17489, .T. ) ;
#14019 = CARTESIAN_POINT ( 'NONE',  ( -7.499999999999994671, -26.00000000000000355, 12.50000000000000000 ) ) ;
#14020 = FACE_BOUND ( 'NONE', #5332, .T. ) ;
#14021 = DIRECTION ( 'NONE',  ( -0.000000000000000000, 0.7071067811865456854, 0.7071067811865493491 ) ) ;
#14022 = FACE_BOUND ( 'NONE', #343, .T. ) ;
#14023 = CARTESIAN_POINT ( 'NONE',  ( -1.265664690411616068E-16, 66.06698730000000808, 47.75000000109246656 ) ) ;
#14024 = ADVANCED_FACE ( 'NONE', ( #18753 ), #1183, .F. ) ;
#14025 = CARTESIAN_POINT ( 'NONE',  ( 2.066987300000001415, 64.85617417291294373, 49.40000000109246514 ) ) ;
#14026 = CARTESIAN_POINT ( 'NONE',  ( 0.000000000000000000, 1.178949249685212974, -2.042000000000001148 ) ) ;
#14027 = EDGE_CURVE ( 'NONE', #16466, #10068, #9995, .T. ) ;
#14028 =( BOUNDED_CURVE ( )  B_SPLINE_CURVE ( 2, ( #7463, #6007, #17963, #18650, #6495, #1887, #17078, #15698, #5025 ),
 .UNSPECIFIED., .F., .F. ) 
 B_SPLINE_CURVE_WITH_KNOTS ( ( 3, 2, 2, 2, 3 ),
 ( 0.000000000000000000, 0.01785714285714280411, 0.03571428571428560822, 0.05357142857142841580, 0.07142857142857121644 ),
 .UNSPECIFIED. ) 
 CURVE ( )  GEOMETRIC_REPRESENTATION_ITEM ( )  RATIONAL_B_SPLINE_CURVE ( ( 1.000000000000000000, 0.9238795325112867385, 1.000000000000000000, 0.9238795325112867385, 1.000000000000000000, 0.9238795325112867385, 1.000000000000000000, 0.9238795325112876267, 0.9999999999999991118 ) ) 
 REPRESENTATION_ITEM ( '' )  );
#14029 = CARTESIAN_POINT ( 'NONE',  ( 2.500000000000001776, 64.00000000000000000, 48.10000000218494165 ) ) ;
#14030 = CARTESIAN_POINT ( 'NONE',  ( -41.00000000000000711, 110.0000000000000000, 14.50000000000000000 ) ) ;
#14031 = VERTEX_POINT ( 'NONE', #9905 ) ;
#14033 = ADVANCED_FACE ( 'NONE', ( #18850 ), #1087, .F. ) ;
#14032 = CARTESIAN_POINT ( 'NONE',  ( -17.35725562635144215, -19.58745947852648683, 30.07617750791695599 ) ) ;
#14034 = LINE ( 'NONE', #9327, #16493 ) ;
#14035 = ORIENTED_EDGE ( 'NONE', *, *, #1964, .F. ) ;
#14036 = CARTESIAN_POINT ( 'NONE',  ( -18.53959229564982536, -27.78091578003890660, 25.26757249208304401 ) ) ;
#14037 = ADVANCED_FACE ( 'NONE', ( #2561 ), #8542, .T. ) ;
#14038 = CARTESIAN_POINT ( 'NONE',  ( -15.96867458239599635, -21.04416526290806999, 32.26757249208305467 ) ) ;
#14039 = DIRECTION ( 'NONE',  ( 0.000000000000000000, 0.000000000000000000, -1.000000000000000000 ) ) ;
#14040 = ORIENTED_EDGE ( 'NONE', *, *, #5328, .F. ) ;
#14041 = LINE ( 'NONE', #3559, #1228 ) ;
#14042 = ORIENTED_EDGE ( 'NONE', *, *, #1596, .F. ) ;
#14043 = CARTESIAN_POINT ( 'NONE',  ( -2.500000000000001776, 64.00000000000000000, 48.50000000218494023 ) ) ;
#14044 = CARTESIAN_POINT ( 'NONE',  ( 0.000000000000000000, 64.00000000000000000, 49.99999999999999289 ) ) ;
#14045 = CIRCLE ( 'NONE', #15294, 2.041999999999999815 ) ;
#14046 = CARTESIAN_POINT ( 'NONE',  ( -2.500000000000001776, 64.00000000000000000, 46.00000000000000000 ) ) ;
#14047 = CARTESIAN_POINT ( 'NONE',  ( -1.461580736456473462, 62.53841926354353120, 45.05000000109246372 ) ) ;
#14048 = EDGE_CURVE ( 'NONE', #3539, #375, #1090, .T. ) ;
#14049 = SURFACE_STYLE_FILL_AREA ( #8181 ) ;
#14050 = LINE ( 'NONE', #9447, #4105 ) ;
#14051 = DIRECTION ( 'NONE',  ( -1.000000000000000000, 0.000000000000000000, -0.000000000000000000 ) ) ;
#14052 = AXIS2_PLACEMENT_3D ( 'NONE', #666, #15936, #17410 ) ;
#14053 = DIRECTION ( 'NONE',  ( -2.973811673103096679E-16, 0.000000000000000000, 1.000000000000000000 ) ) ;
#14054 = VERTEX_POINT ( 'NONE', #898 ) ;
#14055 = CIRCLE ( 'NONE', #2167, 6.000000000000003553 ) ;
#14056 = CARTESIAN_POINT ( 'NONE',  ( -16.17491895705301275, -18.95583473709189803, 30.29492750791695244 ) ) ;
#14057 = CARTESIAN_POINT ( 'NONE',  ( 1.767766952966370653, 62.23223304703363112, 47.20000000218494307 ) ) ;
#14058 = CARTESIAN_POINT ( 'NONE',  ( -10.75228648362912232, -21.35725562635138530, 12.36132249208304046 ) ) ;
#14059 = EDGE_CURVE ( 'NONE', #17432, #3008, #7069, .T. ) ;
#14060 = EDGE_CURVE ( 'NONE', #17940, #18716, #5418, .T. ) ;
#14061 = DIRECTION ( 'NONE',  ( -0.000000000000000000, -1.000000000000000000, -0.000000000000000000 ) ) ;
#14062 = CARTESIAN_POINT ( 'NONE',  ( -11.21908421996108629, -20.46040770435011069, 20.66992750791695244 ) ) ;
#14063 = ADVANCED_FACE ( 'NONE', ( #6096 ), #18155, .T. ) ;
#14064 = LINE ( 'NONE', #12595, #11401 ) ;
#14066 = CARTESIAN_POINT ( 'NONE',  ( -15.16482700510259640, -28.99999999999998224, 33.13867750791696665 ) ) ;
#14065 = VECTOR ( 'NONE', #2451, 1000.000000000000000 ) ;
#14067 = CARTESIAN_POINT ( 'NONE',  ( -41.00000000000000711, 53.00000000000000711, -18.00000000000000000 ) ) ;
#14068 = CARTESIAN_POINT ( 'NONE',  ( -11.46040770435015332, -20.21908421996104011, 22.64257249208304046 ) ) ;
#14069 = CARTESIAN_POINT ( 'NONE',  ( 3.796994071234847710E-16, 61.93301269999999903, 45.95000000109246940 ) ) ;
#14070 = CARTESIAN_POINT ( 'NONE',  ( 0.000000000000000000, 1.178949249685217193, 2.041999999999998483 ) ) ;
#14072 = DIRECTION ( 'NONE',  ( 1.000000000000000000, 0.000000000000000000, 0.000000000000000000 ) ) ;
#14071 = VECTOR ( 'NONE', #995, 1000.000000000000000 ) ;
#14073 = VECTOR ( 'NONE', #11834, 1000.000000000000000 ) ;
#14074 = CARTESIAN_POINT ( 'NONE',  ( -2.500000000000003109, 65.03553390593272354, 48.45000000218494307 ) ) ;
#14075 = CARTESIAN_POINT ( 'NONE',  ( -2.066987300000001415, 63.14382582708705627, 49.00000000109246656 ) ) ;
#14076 = LINE ( 'NONE', #14173, #16795 ) ;
#14077 = ORIENTED_EDGE ( 'NONE', *, *, #18128, .T. ) ;
#14078 = CARTESIAN_POINT ( 'NONE',  ( -8.044165262908093084, -21.95952864787946979, 28.33007249208304756 ) ) ;
#14079 = CIRCLE ( 'NONE', #6579, 6.799999999999999822 ) ;
#14080 = CARTESIAN_POINT ( 'NONE',  ( -10.75228648362912232, -21.35725562635138530, 7.111322492083040459 ) ) ;
#14081 = ADVANCED_FACE ( 'NONE', ( #19329 ), #7268, .T. ) ;
#14082 = CARTESIAN_POINT ( 'NONE',  ( -11.95583473709191047, -23.36097942780921954, 31.60742750791695599 ) ) ;
#14083 = APPLICATION_CONTEXT ( 'automotive_design' ) ;
#14084 = ADVANCED_FACE ( 'NONE', ( #13235 ), #2950, .T. ) ;
#14085 = CARTESIAN_POINT ( 'NONE',  ( -41.00000000000000711, 53.00000000000000711, -11.50000000000000000 ) ) ;
#14086 = CARTESIAN_POINT ( 'NONE',  ( -20.24501739517669563, -18.99630608921239627, 21.33007249208303691 ) ) ;
#14087 = CIRCLE ( 'NONE', #10955, 1.500000000000000222 ) ;
#14088 = CARTESIAN_POINT ( 'NONE',  ( 3.796994071234847710E-16, 61.93301269999999903, 47.35000000109246798 ) ) ;
#14089 = EDGE_LOOP ( 'NONE', ( #7643, #18012, #18122 ) ) ;
#14090 = ORIENTED_EDGE ( 'NONE', *, *, #6133, .F. ) ;
#14091 = CARTESIAN_POINT ( 'NONE',  ( -41.00000000000000711, 110.0000000000000000, -44.00000000000000000 ) ) ;
#14092 = CARTESIAN_POINT ( 'NONE',  ( 0.000000000000000000, 0.7390083445627193548, -1.280000000000000693 ) ) ;
#14093 = AXIS2_PLACEMENT_3D ( 'NONE', #18283, #4852, #9338 ) ;
#14094 = CARTESIAN_POINT ( 'NONE',  ( -0.1250000000000104083, 25.46464466094064250, 60.66708332270462734 ) ) ;
#14095 = FACE_OUTER_BOUND ( 'NONE', #9495, .T. ) ;
#14096 = CARTESIAN_POINT ( 'NONE',  ( -9.551088096457694952E-15, 22.67157287525377996, 59.57106781186547551 ) ) ;
#14097 = VECTOR ( 'NONE', #7092, 1000.000000000000000 ) ;
#14098 = PLANE ( 'NONE',  #16308 ) ;
#14099 = AXIS2_PLACEMENT_3D ( 'NONE', #12039, #7538, #6178 ) ;
#14100 = DIRECTION ( 'NONE',  ( 1.000000000000000000, 0.000000000000000000, 0.000000000000000000 ) ) ;
#14101 = VERTEX_POINT ( 'NONE', #10287 ) ;
#14102 = ORIENTED_EDGE ( 'NONE', *, *, #17086, .T. ) ;
#14103 = CARTESIAN_POINT ( 'NONE',  ( -8.044165262908075320, -26.04047135212042718, 26.79492750791695954 ) ) ;
#14104 = ORIENTED_EDGE ( 'NONE', *, *, #1714, .F. ) ;
#14105 = VECTOR ( 'NONE', #3955, 1000.000000000000000 ) ;
#14107 = ORIENTED_EDGE ( 'NONE', *, *, #5891, .F. ) ;
#14106 = VERTEX_POINT ( 'NONE', #12157 ) ;
#14108 = EDGE_CURVE ( 'NONE', #5479, #6083, #8926, .T. ) ;
#14109 = CARTESIAN_POINT ( 'NONE',  ( -14.36097942780925685, -20.95583473709189093, 27.45507249208304756 ) ) ;
#14110 = CARTESIAN_POINT ( 'NONE',  ( -7.955834737091916686, -22.28918265808470522, 15.85742750791695954 ) ) ;
#14111 = CIRCLE ( 'NONE', #8776, 0.1000000000000000472 ) ;
#14112 = CARTESIAN_POINT ( 'NONE',  ( 1.767766952966369987, 65.76776695296638309, 47.29999999999999716 ) ) ;
#14113 = CARTESIAN_POINT ( 'NONE',  ( -1.767766952966370209, 65.76776695296638309, 48.40000000218494591 ) ) ;
#14114 = CARTESIAN_POINT ( 'NONE',  ( 5.199999999999996625, 0.000000000000000000, 2.500000000000000444 ) ) ;
#14115 = ORIENTED_EDGE ( 'NONE', *, *, #8549, .T. ) ;
#14116 = CARTESIAN_POINT ( 'NONE',  ( -18.04416526290808420, -24.63902057219074493, 23.73242750791696665 ) ) ;
#14117 = VECTOR ( 'NONE', #16530, 1000.000000000000000 ) ;
#14118 = CARTESIAN_POINT ( 'NONE',  ( -0.9999999999999945599, -36.00000000000000711, 9.500000000000001776 ) ) ;
#14119 = ORIENTED_EDGE ( 'NONE', *, *, #15317, .T. ) ;
#14120 = DIRECTION ( 'NONE',  ( -1.000000000000000000, -0.000000000000000000, -0.000000000000000000 ) ) ;
#14121 = ORIENTED_EDGE ( 'NONE', *, *, #259, .F. ) ;
#14122 = FACE_OUTER_BOUND ( 'NONE', #3750, .T. ) ;
#14123 = CARTESIAN_POINT ( 'NONE',  ( -1.767766952966369765, 62.23223304703363112, 45.29999999999999005 ) ) ;
#14124 = DIRECTION ( 'NONE',  ( 0.000000000000000000, -1.000000000000000000, -0.000000000000000000 ) ) ;
#14125 = CARTESIAN_POINT ( 'NONE',  ( -1.265664690411616068E-16, 66.06698730000000808, 49.35000000109246798 ) ) ;
#14126 = MECHANICAL_DESIGN_GEOMETRIC_PRESENTATION_REPRESENTATION (  '', ( #5977 ), #12239 ) ;
#14127 = CARTESIAN_POINT ( 'NONE',  ( 0.8561741729129460632, 66.06698730000000808, 47.90000000109247225 ) ) ;
#14128 = DIRECTION ( 'NONE',  ( -0.000000000000000000, -1.000000000000000000, -0.000000000000000000 ) ) ;
#14129 = VECTOR ( 'NONE', #18574, 1000.000000000000000 ) ;
#14130 = DIRECTION ( 'NONE',  ( -0.000000000000000000, -1.000000000000000000, -0.000000000000000000 ) ) ;
#14131 = CARTESIAN_POINT ( 'NONE',  ( 1.865360897248530714, 62.81633110618239613, 45.00000000000000711 ) ) ;
#14132 = ORIENTED_EDGE ( 'NONE', *, *, #6997, .T. ) ;
#14133 = CARTESIAN_POINT ( 'NONE',  ( -12.64274437364855252, -28.41254052147347053, 27.45117750791695954 ) ) ;
#14134 = CIRCLE ( 'NONE', #13160, 2.500000000000002220 ) ;
#14135 = DIRECTION ( 'NONE',  ( 0.000000000000000000, 1.000000000000000000, -1.471414886128461669E-15 ) ) ;
#14136 = ORIENTED_EDGE ( 'NONE', *, *, #4853, .T. ) ;
#14137 = CARTESIAN_POINT ( 'NONE',  ( -10.04416526290808953, -22.49542703274172695, 38.83007249208302625 ) ) ;
#14138 = CARTESIAN_POINT ( 'NONE',  ( -25.00000000000000000, 53.00000000000000711, 26.50000000000000000 ) ) ;
#14139 = CARTESIAN_POINT ( 'NONE',  ( -11.95583473709190514, -24.63902057219072361, 39.26757249208304756 ) ) ;
#14140 = CARTESIAN_POINT ( 'NONE',  ( -31.74999999999995737, 0.000000000000000000, 0.000000000000000000 ) ) ;
#14141 = ORIENTED_EDGE ( 'NONE', *, *, #15282, .T. ) ;
#14142 = VECTOR ( 'NONE', #358, 1000.000000000000000 ) ;
#14143 = DIRECTION ( 'NONE',  ( -1.000000000000000000, -0.000000000000000000, -0.000000000000000000 ) ) ;
#14144 = ORIENTED_EDGE ( 'NONE', *, *, #18596, .T. ) ;
#14145 = CARTESIAN_POINT ( 'NONE',  ( 24.99999999999998579, -6.000000000000000000, 42.49999999999997868 ) ) ;
#14146 = DIRECTION ( 'NONE',  ( -1.000000000000000000, 0.000000000000000000, -0.000000000000000000 ) ) ;
#14147 =( BOUNDED_CURVE ( )  B_SPLINE_CURVE ( 2, ( #3815, #15583, #2151, #8139, #6211, #771, #14112, #12723, #17335 ),
 .UNSPECIFIED., .F., .F. ) 
 B_SPLINE_CURVE_WITH_KNOTS ( ( 3, 2, 2, 2, 3 ),
 ( 0.4285714285714284921, 0.4464285714285714524, 0.4642857142857143016, 0.4821428571428572063, 0.5000000000000001110 ),
 .UNSPECIFIED. ) 
 CURVE ( )  GEOMETRIC_REPRESENTATION_ITEM ( )  RATIONAL_B_SPLINE_CURVE ( ( 1.000000000000000222, 0.9238795325112865164, 1.000000000000000000, 0.9238795325112867385, 1.000000000000000000, 0.9238795325112867385, 1.000000000000000000, 0.9238795325112862944, 1.000000000000000444 ) ) 
 REPRESENTATION_ITEM ( '' )  );
#14148 = AXIS2_PLACEMENT_3D ( 'NONE', #3565, #340, #10810 ) ;
#14149 = LINE ( 'NONE', #15326, #10358 ) ;
#14150 = DIRECTION ( 'NONE',  ( 0.000000000000000000, -1.000000000000000000, 0.000000000000000000 ) ) ;
#14151 = DIRECTION ( 'NONE',  ( 0.000000000000000000, 0.000000000000000000, -1.000000000000000000 ) ) ;
#14152 = PLANE ( 'NONE',  #13327 ) ;
#14153 = LINE ( 'NONE', #16532, #18965 ) ;
#14154 = UNCERTAINTY_MEASURE_WITH_UNIT (LENGTH_MEASURE( 1.000000000000000082E-05 ), #15196, 'distance_accuracy_value', 'NONE');
#14155 = ORIENTED_EDGE ( 'NONE', *, *, #2081, .T. ) ;
#14156 = VECTOR ( 'NONE', #5109, 1000.000000000000000 ) ;
#14157 = CARTESIAN_POINT ( 'NONE',  ( -9.955834737091912245, -22.82508104294696594, 26.35742750791695954 ) ) ;
#14158 = CARTESIAN_POINT ( 'NONE',  ( -1.767766952966369765, 62.23223304703363112, 47.00000000218494733 ) ) ;
#14159 = EDGE_CURVE ( 'NONE', #578, #9204, #9128, .T. ) ;
#14160 = ADVANCED_FACE ( 'NONE', ( #9025 ), #7458, .T. ) ;
#14161 = CARTESIAN_POINT ( 'NONE',  ( -16.50457296725825174, -19.04416526290807354, 37.51757249208304046 ) ) ;
#14162 = CARTESIAN_POINT ( 'NONE',  ( 0.000000000000000000, 52.00000000000000711, 30.00000000000000000 ) ) ;
#14163 = CARTESIAN_POINT ( 'NONE',  ( -19.41254052147348830, -26.35725562635142083, 28.76367750791695954 ) ) ;
#14164 = DIRECTION ( 'NONE',  ( 0.000000000000000000, 0.000000000000000000, -1.000000000000000000 ) ) ;
#14165 = CARTESIAN_POINT ( 'NONE',  ( -9.955834737091912245, -22.82508104294696238, 26.35742750791695599 ) ) ;
#14166 = DIRECTION ( 'NONE',  ( -1.000000000000000000, -0.000000000000000000, -0.000000000000000000 ) ) ;
#14167 = CARTESIAN_POINT ( 'NONE',  ( -18.53959229564983247, -27.78091578003891016, 25.26757249208304401 ) ) ;
#14168 = CARTESIAN_POINT ( 'NONE',  ( -1.767766952966369765, 62.23223304703363112, 48.49999999999999289 ) ) ;
#14169 = CARTESIAN_POINT ( 'NONE',  ( 2.500000000000001776, 64.00000000000000000, 47.99999999999999289 ) ) ;
#14170 = CARTESIAN_POINT ( 'NONE',  ( -37.50000000000002132, 0.000000000000000000, 44.99999999999997868 ) ) ;
#14171 = DIRECTION ( 'NONE',  ( 0.000000000000000000, 0.000000000000000000, -1.000000000000000000 ) ) ;
#14172 = CARTESIAN_POINT ( 'NONE',  ( 1.035533905932739751, 61.50000000000000000, 48.64999999999999858 ) ) ;
#14173 = CARTESIAN_POINT ( 'NONE',  ( -41.00000000000000711, 53.00000000000000711, 1.500000000000001332 ) ) ;
#14174 = ADVANCED_FACE ( 'NONE', ( #16386 ), #11965, .T. ) ;
#14175 = CLOSED_SHELL ( 'NONE', ( #17577, #17482, #18505, #6544, #16807, #5095, #8511, #9193, #9965, #6998, #17332, #14174, #6598, #7266, #17002, #17149, #12278, #13409, #1060, #2326, #1413, #14547, #2453, #1366, #9258, #17173, #15851, #12607, #16709, #2902, #13528, #3610, #169, #17385, #1851, #14160, #190, #17046, #4081, #16132, #13176, #4607, #14063, #15717, #56 ) ) ;
#14176 = ORIENTED_EDGE ( 'NONE', *, *, #3157, .F. ) ;
#14177 = EDGE_CURVE ( 'NONE', #1682, #663, #12060, .T. ) ;
#14178 = EDGE_CURVE ( 'NONE', #9439, #19394, #10489, .T. ) ;
#14179 =( NAMED_UNIT ( * ) PLANE_ANGLE_UNIT ( ) SI_UNIT ( $, .RADIAN. ) );
#14180 = DIRECTION ( 'NONE',  ( 0.000000000000000000, 0.000000000000000000, 1.000000000000000000 ) ) ;
#14181 = CARTESIAN_POINT ( 'NONE',  ( -12.68318583509884157, -21.92450931948787485, 25.91992750791696309 ) ) ;
#14182 = CARTESIAN_POINT ( 'NONE',  ( 43.50000000000001421, 115.0000000000000000, 32.49999999999998579 ) ) ;
#14183 = CARTESIAN_POINT ( 'NONE',  ( -21.14459132904239169, -20.64274437364858628, 36.86132249208304046 ) ) ;
#14184 = CARTESIAN_POINT ( 'NONE',  ( 1.461580736456473906, 62.53841926354353120, 46.65000000109247225 ) ) ;
#14185 = ORIENTED_EDGE ( 'NONE', *, *, #7349, .F. ) ;
#14186 = VERTEX_POINT ( 'NONE', #7661 ) ;
#14187 = DIRECTION ( 'NONE',  ( 0.000000000000000000, -0.7071067811865493491, 0.7071067811865457964 ) ) ;
#14188 = CARTESIAN_POINT ( 'NONE',  ( -2.500000000000001776, 64.00000000000000000, 46.90000000218494591 ) ) ;
#14189 = CARTESIAN_POINT ( 'NONE',  ( 2.066987300000001415, 64.85617417291294373, 45.20000000109248361 ) ) ;
#14190 = CARTESIAN_POINT ( 'NONE',  ( 0.000000000000000000, 64.00000000000000000, 49.99999999999999289 ) ) ;
#14191 = CARTESIAN_POINT ( 'NONE',  ( -1.767766952966370209, 65.76776695296638309, 49.89999999999999147 ) ) ;
#14192 = DIRECTION ( 'NONE',  ( 0.000000000000000000, -1.000000000000000000, 0.000000000000000000 ) ) ;
#14193 = EDGE_CURVE ( 'NONE', #10900, #1798, #16486, .T. ) ;
#14194 = LINE ( 'NONE', #10049, #14272 ) ;
#14195 = ORIENTED_EDGE ( 'NONE', *, *, #1360, .T. ) ;
#14196 = EDGE_LOOP ( 'NONE', ( #4754, #2553, #17637, #16667 ) ) ;
#14197 = CARTESIAN_POINT ( 'NONE',  ( -8.855408670957631401, -20.64274437364852943, 36.63867750791695244 ) ) ;
#14198 =( NAMED_UNIT ( * ) SI_UNIT ( $, .STERADIAN. ) SOLID_ANGLE_UNIT ( ) );
#14199 = ORIENTED_EDGE ( 'NONE', *, *, #3536, .T. ) ;
#14201 = VERTEX_POINT ( 'NONE', #15011 ) ;
#14200 = EDGE_LOOP ( 'NONE', ( #8617, #8028 ) ) ;
#14202 = CARTESIAN_POINT ( 'NONE',  ( -16.35725562635141372, -26.68048971390461332, 30.29882249208304401 ) ) ;
#14203 = ADVANCED_FACE ( 'NONE', ( #1588 ), #13536, .F. ) ;
#14204 = CARTESIAN_POINT ( 'NONE',  ( -7.955834737091916686, -22.28918265808470522, 21.10742750791695954 ) ) ;
#14205 = LINE ( 'NONE', #11154, #14767 ) ;
#14206 = CARTESIAN_POINT ( 'NONE',  ( -2.500000000000000888, 62.96446609406726935, 48.55000000218494449 ) ) ;
#14207 = FACE_OUTER_BOUND ( 'NONE', #7315, .T. ) ;
#14208 = ORIENTED_EDGE ( 'NONE', *, *, #16596, .T. ) ;
#14209 = CARTESIAN_POINT ( 'NONE',  ( -12.48433729119798130, -25.64274437364855075, 32.26367750791695954 ) ) ;
#14210 = LINE ( 'NONE', #8604, #13165 ) ;
#14211 = EDGE_LOOP ( 'NONE', ( #694, #17327, #4016, #101 ) ) ;
#14212 = LINE ( 'NONE', #8245, #17854 ) ;
#14213 = ORIENTED_EDGE ( 'NONE', *, *, #12665, .F. ) ;
#14214 = CARTESIAN_POINT ( 'NONE',  ( -0.6673928701031922595, 62.03906428592985378, 45.00000000000002132 ) ) ;
#14215 = CARTESIAN_POINT ( 'NONE',  ( 0.000000000000000000, 64.00000000000000000, 49.99999999999999289 ) ) ;
#14216 = LINE ( 'NONE', #12452, #16908 ) ;
#14217 = CARTESIAN_POINT ( 'NONE',  ( 2.066987300000001859, 64.85617417291294373, 48.40000000109247225 ) ) ;
#14218 = EDGE_CURVE ( 'NONE', #1789, #3990, #4329, .T. ) ;
#14219 = CARTESIAN_POINT ( 'NONE',  ( -2.066987300000001415, 64.85617417291294373, 48.90000000109247225 ) ) ;
#14220 = LINE ( 'NONE', #8155, #15053 ) ;
#14221 = CARTESIAN_POINT ( 'NONE',  ( 4.999999999999993783, 68.00000000000000000, 69.99999999999998579 ) ) ;
#14222 = CARTESIAN_POINT ( 'NONE',  ( 2.314696032948281967, 63.84105539985402089, 44.99999999999999289 ) ) ;
#14223 = VERTEX_POINT ( 'NONE', #8725 ) ;
#14224 = VERTEX_POINT ( 'NONE', #18060 ) ;
#14225 = CARTESIAN_POINT ( 'NONE',  ( -10.58745947852649927, -21.64274437364853654, 36.63867750791695954 ) ) ;
#14226 = CYLINDRICAL_SURFACE ( 'NONE', #12430, 2.999999999999999112 ) ;
#14227 = ORIENTED_EDGE ( 'NONE', *, *, #1596, .T. ) ;
#14228 = AXIS2_PLACEMENT_3D ( 'NONE', #17891, #11893, #17684 ) ;
#14229 = CARTESIAN_POINT ( 'NONE',  ( -19.24771351637086880, -26.64274437364857206, 30.73632249208304401 ) ) ;
#14230 = CARTESIAN_POINT ( 'NONE',  ( -41.00000000000000711, 110.0000000000000000, -45.00000000000000000 ) ) ;
#14231 = CARTESIAN_POINT ( 'NONE',  ( -13.35725562635141195, -26.51566270880198672, 34.67382249208304756 ) ) ;
#14232 = DIRECTION ( 'NONE',  ( 1.000000000000000000, -0.000000000000000000, -0.000000000000000000 ) ) ;
#14233 = ORIENTED_EDGE ( 'NONE', *, *, #7832, .T. ) ;
#14234 = DIRECTION ( 'NONE',  ( -1.000000000000000000, 2.665111688417744333E-15, -2.272588573746785565E-15 ) ) ;
#14235 = ORIENTED_EDGE ( 'NONE', *, *, #11623, .T. ) ;
#14236 = CARTESIAN_POINT ( 'NONE',  ( -7.999999999999996447, 0.000000000000000000, 1.500000000000000000 ) ) ;
#14237 = DIRECTION ( 'NONE',  ( -0.000000000000000000, -0.000000000000000000, -1.000000000000000000 ) ) ;
#14238 = DIRECTION ( 'NONE',  ( -0.000000000000000000, -1.000000000000000000, -0.000000000000000000 ) ) ;
#14239 = AXIS2_PLACEMENT_3D ( 'NONE', #13158, #14538, #18767 ) ;
#14240 = CARTESIAN_POINT ( 'NONE',  ( -8.528048594804062077, -42.28611686177728046, 3.000000000000000000 ) ) ;
#14241 = DIRECTION ( 'NONE',  ( 0.7071067811865535679, 0.4999999999999973355, -0.4999999999999940048 ) ) ;
#14242 = DIRECTION ( 'NONE',  ( 0.000000000000000000, -1.000000000000000000, 0.000000000000000000 ) ) ;
#14243 = DIRECTION ( 'NONE',  ( 2.602085213965211135E-16, -1.000000000000000000, 0.000000000000000000 ) ) ;
#14244 = ORIENTED_EDGE ( 'NONE', *, *, #17493, .T. ) ;
#14245 = DIRECTION ( 'NONE',  ( 0.000000000000000000, 0.7071067811865492381, -0.7071067811865456854 ) ) ;
#14246 = CARTESIAN_POINT ( 'NONE',  ( -12.64274437364855252, -28.41254052147347053, 32.70117750791696665 ) ) ;
#14247 = CARTESIAN_POINT ( 'NONE',  ( 0.8561741729129460632, 66.06698729999999387, 47.70000000109248361 ) ) ;
#14248 = CARTESIAN_POINT ( 'NONE',  ( -10.75228648362912232, -21.35725562635138530, 38.61132249208304046 ) ) ;
#14249 =( BOUNDED_CURVE ( )  B_SPLINE_CURVE ( 2, ( #5968, #11728, #17930, #5672, #16248, #16550, #17627, #16451, #6067 ),
 .UNSPECIFIED., .F., .F. ) 
 B_SPLINE_CURVE_WITH_KNOTS ( ( 3, 2, 2, 2, 3 ),
 ( 0.6428571428571427937, 0.6607142857142855874, 0.6785714285714284921, 0.6964285714285712858, 0.7142857142857141906 ),
 .UNSPECIFIED. ) 
 CURVE ( )  GEOMETRIC_REPRESENTATION_ITEM ( )  RATIONAL_B_SPLINE_CURVE ( ( 1.000000000000000444, 0.9238795325112862944, 1.000000000000000000, 0.9238795325112867385, 1.000000000000000000, 0.9238795325112867385, 1.000000000000000000, 0.9238795325112871826, 0.9999999999999995559 ) ) 
 REPRESENTATION_ITEM ( '' )  );
#14250 = DIRECTION ( 'NONE',  ( -1.000000000000000000, -0.000000000000000000, -0.000000000000000000 ) ) ;
#14251 = CARTESIAN_POINT ( 'NONE',  ( -17.64274437364855430, -28.24771351637087236, 28.32617750791695954 ) ) ;
#14252 = LINE ( 'NONE', #18398, #7996 ) ;
#14253 = CARTESIAN_POINT ( 'NONE',  ( -18.78091578003889595, -27.53959229564985023, 33.79492750791695954 ) ) ;
#14254 = CARTESIAN_POINT ( 'NONE',  ( 0.1499999999999973577, 3.184081677783118191E-16, -2.600000000000000089 ) ) ;
#14255 = CARTESIAN_POINT ( 'NONE',  ( -19.99999999999999645, -24.16482700510261949, 31.17382249208304046 ) ) ;
#14256 = CARTESIAN_POINT ( 'NONE',  ( -2.500000000000001776, 65.03553390593273775, 48.35000000000000142 ) ) ;
#14257 = CARTESIAN_POINT ( 'NONE',  ( 0.08838834764830767743, 29.68014068711926257, 56.80514068711929809 ) ) ;
#14258 = AXIS2_PLACEMENT_3D ( 'NONE', #7874, #6496, #15420 ) ;
#14259 = AXIS2_PLACEMENT_3D ( 'NONE', #10647, #16650, #8795 ) ;
#14260 = FACE_OUTER_BOUND ( 'NONE', #13218, .T. ) ;
#14261 = CARTESIAN_POINT ( 'NONE',  ( -1.767766952966369765, 62.23223304703363112, 48.49999999999999289 ) ) ;
#14262 = EDGE_CURVE ( 'NONE', #4388, #5200, #13628, .T. ) ;
#14263 = EDGE_CURVE ( 'NONE', #8981, #8886, #6201, .T. ) ;
#14264 = DIRECTION ( 'NONE',  ( 0.000000000000000000, -0.5000000000000013323, -0.8660254037844380415 ) ) ;
#14265 = ORIENTED_EDGE ( 'NONE', *, *, #3776, .T. ) ;
#14266 = ADVANCED_FACE ( 'NONE', ( #1684 ), #214, .F. ) ;
#14267 = CARTESIAN_POINT ( 'NONE',  ( -0.8561741729129466183, 61.93301270000000613, 44.90000000109247225 ) ) ;
#14268 = CARTESIAN_POINT ( 'NONE',  ( -13.49542703274178379, -19.04416526290806289, 4.482427507916957765 ) ) ;
#14269 = PLANE ( 'NONE',  #8221 ) ;
#14270 = EDGE_CURVE ( 'NONE', #3008, #5563, #10979, .T. ) ;
#14271 = CARTESIAN_POINT ( 'NONE',  ( -7.955834737091903364, -25.71081734191518464, 39.26757249208304756 ) ) ;
#14272 = VECTOR ( 'NONE', #17809, 1000.000000000000000 ) ;
#14273 = VECTOR ( 'NONE', #4063, 1000.000000000000114 ) ;
#14274 = CARTESIAN_POINT ( 'NONE',  ( 2.066987300000001859, 64.85617417291294373, 45.20000000109248361 ) ) ;
#14275 = EDGE_LOOP ( 'NONE', ( #6377, #11402, #2423, #17582 ) ) ;
#14276 = DIRECTION ( 'NONE',  ( -1.156482317317871478E-16, 1.000000000000000000, 0.000000000000000000 ) ) ;
#14277 = LINE ( 'NONE', #3982, #12257 ) ;
#14278 = DIRECTION ( 'NONE',  ( 1.000000000000000000, -0.000000000000000000, -0.000000000000000000 ) ) ;
#14279 = LINE ( 'NONE', #15940, #11211 ) ;
#14280 = FACE_OUTER_BOUND ( 'NONE', #1800, .T. ) ;
#14281 = CARTESIAN_POINT ( 'NONE',  ( 2.500000000000007994, 62.96446609406726225, 48.74999999999999289 ) ) ;
#14282 = AXIS2_PLACEMENT_3D ( 'NONE', #12069, #4642, #11870 ) ;
#14283 = AXIS2_PLACEMENT_3D ( 'NONE', #7967, #11260, #2168 ) ;
#14284 = CARTESIAN_POINT ( 'NONE',  ( 34.99999999999999289, -6.000000000000000000, 42.49999999999997868 ) ) ;
#14285 = ORIENTED_EDGE ( 'NONE', *, *, #11868, .T. ) ;
#14286 = VERTEX_POINT ( 'NONE', #18450 ) ;
#14287 = CARTESIAN_POINT ( 'NONE',  ( -22.04416526290807710, -25.71081734191525925, 39.48242750791695244 ) ) ;
#14288 =( LENGTH_UNIT ( ) NAMED_UNIT ( * ) SI_UNIT ( .MILLI., .METRE. ) );
#14289 = ORIENTED_EDGE ( 'NONE', *, *, #1024, .T. ) ;
#14291 = ORIENTED_EDGE ( 'NONE', *, *, #11675, .T. ) ;
#14290 = EDGE_LOOP ( 'NONE', ( #8118, #10374, #12296 ) ) ;
#14292 = CARTESIAN_POINT ( 'NONE',  ( -12.31951028609536536, -25.35725562635139596, 28.98632249208304401 ) ) ;
#14293 = CARTESIAN_POINT ( 'NONE',  ( -20.00369391078762860, -18.75498260482333279, 24.60742750791696309 ) ) ;
#14294 = FACE_OUTER_BOUND ( 'NONE', #16846, .T. ) ;
#14295 = CARTESIAN_POINT ( 'NONE',  ( 2.500000000000001776, 64.00000000000000000, 48.10000000218494165 ) ) ;
#14296 = PLANE ( 'NONE',  #4383 ) ;
#14297 = VERTEX_POINT ( 'NONE', #15500 ) ;
#14298 = VECTOR ( 'NONE', #199, 1000.000000000000000 ) ;
#14299 = CARTESIAN_POINT ( 'NONE',  ( -24.00000000000000711, 53.00000000000000711, -45.00000000000000000 ) ) ;
#14300 = EDGE_LOOP ( 'NONE', ( #15770, #18334, #19153, #4599 ) ) ;
#14301 = ADVANCED_FACE ( 'NONE', ( #9417 ), #18354, .F. ) ;
#14302 = EDGE_CURVE ( 'NONE', #3842, #853, #309, .T. ) ;
#14303 = DIRECTION ( 'NONE',  ( -1.000000000000000000, 0.000000000000000000, -0.000000000000000000 ) ) ;
#14304 = ORIENTED_EDGE ( 'NONE', *, *, #18855, .F. ) ;
#14305 = DIRECTION ( 'NONE',  ( -0.000000000000000000, -0.000000000000000000, -1.000000000000000000 ) ) ;
#14306 = DIRECTION ( 'NONE',  ( -0.000000000000000000, -0.000000000000000000, -1.000000000000000000 ) ) ;
#14307 = PLANE ( 'NONE',  #9376 ) ;
#14308 = ADVANCED_FACE ( 'NONE', ( #12555 ), #10884, .T. ) ;
#14309 = CARTESIAN_POINT ( 'NONE',  ( -0.8561741729129461742, 66.06698729999999387, 47.00000000109247367 ) ) ;
#14310 = ADVANCED_FACE ( 'NONE', ( #16686 ), #3443, .F. ) ;
#14311 = PLANE ( 'NONE',  #15363 ) ;
#14312 = DIRECTION ( 'NONE',  ( -1.000000000000000000, 0.000000000000000000, -0.000000000000000000 ) ) ;
#14313 = ORIENTED_EDGE ( 'NONE', *, *, #14048, .F. ) ;
#14314 = ORIENTED_EDGE ( 'NONE', *, *, #11267, .T. ) ;
#14315 = CARTESIAN_POINT ( 'NONE',  ( -10.75228648362910100, -26.64274437364854009, 32.26367750791695954 ) ) ;
#14316 = FACE_OUTER_BOUND ( 'NONE', #7981, .T. ) ;
#14317 = EDGE_LOOP ( 'NONE', ( #11819, #19191, #7362, #11172 ) ) ;
#14318 = CARTESIAN_POINT ( 'NONE',  ( -16.50457296725825174, -19.04416526290807354, 32.26757249208304046 ) ) ;
#14319 = CARTESIAN_POINT ( 'NONE',  ( 2.500000000000001776, 64.00000000000000000, 48.90000000218494591 ) ) ;
#14320 = EDGE_CURVE ( 'NONE', #11555, #16697, #15506, .T. ) ;
#14321 = EDGE_CURVE ( 'NONE', #6553, #16539, #16984, .T. ) ;
#14322 = ORIENTED_EDGE ( 'NONE', *, *, #9946, .F. ) ;
#14323 = CARTESIAN_POINT ( 'NONE',  ( -15.16482700510262482, -20.99999999999997513, 32.48632249208304756 ) ) ;
#14324 = DIRECTION ( 'NONE',  ( -1.000000000000000000, 0.000000000000000000, -0.000000000000000000 ) ) ;
#14325 = VERTEX_POINT ( 'NONE', #18554 ) ;
#14326 = CARTESIAN_POINT ( 'NONE',  ( 44.99999999999997158, 3.000000000000000000, 55.00000000000000000 ) ) ;
#14327 = ORIENTED_EDGE ( 'NONE', *, *, #15896, .F. ) ;
#14328 = DIRECTION ( 'NONE',  ( -1.000000000000000000, 0.000000000000000000, -0.000000000000000000 ) ) ;
#14329 = DIRECTION ( 'NONE',  ( 0.000000000000000000, 1.000000000000000000, -0.000000000000000000 ) ) ;
#14330 = DIRECTION ( 'NONE',  ( 1.000000000000000000, -0.000000000000000000, -0.000000000000000000 ) ) ;
#14331 = SURFACE_STYLE_FILL_AREA ( #2285 ) ;
#14332 = PLANE ( 'NONE',  #16809 ) ;
#14333 = CARTESIAN_POINT ( 'NONE',  ( 11.83926609531033058, -43.78611686177728046, 3.000000000000000000 ) ) ;
#14334 = ORIENTED_EDGE ( 'NONE', *, *, #8229, .F. ) ;
#14335 = ORIENTED_EDGE ( 'NONE', *, *, #436, .T. ) ;
#14336 = CARTESIAN_POINT ( 'NONE',  ( -19.95583473709191580, -22.49542703274176603, 29.41992750791695599 ) ) ;
#14337 = EDGE_CURVE ( 'NONE', #13388, #1370, #3354, .T. ) ;
#14338 = CARTESIAN_POINT ( 'NONE',  ( 2.066987300000001415, 64.00000000000000000, 49.15000000109247225 ) ) ;
#14339 = CARTESIAN_POINT ( 'NONE',  ( -15.16482700510263371, -18.99999999999997868, 27.23632249208304046 ) ) ;
#14340 = AXIS2_PLACEMENT_3D ( 'NONE', #6532, #3583, #13777 ) ;
#14341 = CARTESIAN_POINT ( 'NONE',  ( 2.315774708385922587, 27.80336399182260720, 58.32836399182267684 ) ) ;
#14342 = LINE ( 'NONE', #7182, #2486 ) ;
#14343 = CARTESIAN_POINT ( 'NONE',  ( -14.83517299489739649, -18.99999999999997868, 25.26367750791695599 ) ) ;
#14344 = CARTESIAN_POINT ( 'NONE',  ( -15.00000000000000000, -35.74454190283287147, 7.499999999999995559 ) ) ;
#14345 = CARTESIAN_POINT ( 'NONE',  ( -19.41254052147348830, -26.35725562635142083, 28.76367750791695954 ) ) ;
#14346 = CARTESIAN_POINT ( 'NONE',  ( -1.767766952966370209, 65.76776695296638309, 46.80000000218494449 ) ) ;
#14347 = CARTESIAN_POINT ( 'NONE',  ( -10.58745947852648328, -26.35725562635138530, 39.48632249208304046 ) ) ;
#14348 = CARTESIAN_POINT ( 'NONE',  ( 1.035533905932738197, 66.50000000000000000, 48.94999999999999574 ) ) ;
#14349 = CARTESIAN_POINT ( 'NONE',  ( -2.066987300000001415, 64.85617417291294373, 48.90000000109247225 ) ) ;
#14350 = DIRECTION ( 'NONE',  ( 0.000000000000000000, -1.000000000000000000, 0.000000000000000000 ) ) ;
#14351 = CARTESIAN_POINT ( 'NONE',  ( 1.461580736456473906, 62.53841926354353120, 46.05000000109246372 ) ) ;
#14352 = DIRECTION ( 'NONE',  ( 0.000000000000000000, 1.000000000000000000, 0.000000000000000000 ) ) ;
#14353 = CIRCLE ( 'NONE', #7473, 1.500000000000000222 ) ;
#14354 = ORIENTED_EDGE ( 'NONE', *, *, #7976, .F. ) ;
#14355 = ADVANCED_FACE ( 'NONE', ( #501, #12265, #5020, #1880, #6489, #9512, #14022, #593, #5123, #11076, #13729, #10688, #15213 ), #7764, .F. ) ;
#14356 = CARTESIAN_POINT ( 'NONE',  ( -24.00000000000000000, 53.00000000000000711, 6.999999999999999112 ) ) ;
#14357 = ADVANCED_FACE ( 'NONE', ( #15304 ), #13833, .T. ) ;
#14358 = CARTESIAN_POINT ( 'NONE',  ( -16.35725562635142794, -21.31951028609535470, 40.57617750791696665 ) ) ;
#14359 = FACE_OUTER_BOUND ( 'NONE', #5877, .T. ) ;
#14360 = CARTESIAN_POINT ( 'NONE',  ( -7.955834737091903364, -25.71081734191518464, 34.01757249208303335 ) ) ;
#14361 = VECTOR ( 'NONE', #16252, 1000.000000000000000 ) ;
#14362 = CARTESIAN_POINT ( 'NONE',  ( 2.066987300000002303, 63.14382582708705627, 49.30000000109246372 ) ) ;
#14363 = EDGE_LOOP ( 'NONE', ( #16681, #1357, #13311, #10645 ) ) ;
#14364 = AXIS2_PLACEMENT_3D ( 'NONE', #18553, #8249, #9511 ) ;
#14365 = DIRECTION ( 'NONE',  ( -0.000000000000000000, -0.000000000000000000, -1.000000000000000000 ) ) ;
#14366 = CARTESIAN_POINT ( 'NONE',  ( -41.00000000000000711, 110.0000000000000000, 26.50000000000000000 ) ) ;
#14367 = CARTESIAN_POINT ( 'NONE',  ( -1.265664690411616068E-16, 66.06698730000000808, 47.75000000109246656 ) ) ;
#14368 = CARTESIAN_POINT ( 'NONE',  ( -4.012830983233701687, 26.60336399182265055, 59.52836399182262994 ) ) ;
#14369 = CARTESIAN_POINT ( 'NONE',  ( 1.767766952966369987, 65.76776695296638309, 49.00000000218494023 ) ) ;
#14370 = CARTESIAN_POINT ( 'NONE',  ( -41.00000000000000000, 0.000000000000000000, 30.00000000000000000 ) ) ;
#14371 = AXIS2_PLACEMENT_3D ( 'NONE', #18279, #7683, #15523 ) ;
#14372 = LINE ( 'NONE', #11231, #16143 ) ;
#14373 = ORIENTED_EDGE ( 'NONE', *, *, #14871, .F. ) ;
#14374 = VERTEX_POINT ( 'NONE', #7627 ) ;
#14375 = CARTESIAN_POINT ( 'NONE',  ( -9.754982604823302594, -29.00369391078756465, 8.205072492083040459 ) ) ;
#14376 = EDGE_CURVE ( 'NONE', #10477, #763, #3604, .T. ) ;
#14377 = VECTOR ( 'NONE', #15430, 1000.000000000000000 ) ;
#14378 = EDGE_LOOP ( 'NONE', ( #19327, #3551, #17723, #324 ) ) ;
#14379 = VECTOR ( 'NONE', #7738, 1000.000000000000114 ) ;
#14381 = ORIENTED_EDGE ( 'NONE', *, *, #2678, .F. ) ;
#14380 = EDGE_LOOP ( 'NONE', ( #1396, #3030, #12027, #1477 ) ) ;
#14382 = CARTESIAN_POINT ( 'NONE',  ( -11.99999999999999289, -23.83517299489735564, 39.04882249208304756 ) ) ;
#14383 = CARTESIAN_POINT ( 'NONE',  ( -8.855408670957631401, -20.64274437364852943, 31.38867750791695599 ) ) ;
#14384 = VECTOR ( 'NONE', #5285, 1000.000000000000114 ) ;
#14385 = FACE_OUTER_BOUND ( 'NONE', #11727, .T. ) ;
#14386 = CARTESIAN_POINT ( 'NONE',  ( -1.767766952966370209, 65.76776695296638309, 47.60000000218494165 ) ) ;
#14387 = CARTESIAN_POINT ( 'NONE',  ( -44.99999999999998579, 3.000000000000000000, -55.00000000000000000 ) ) ;
#14388 = ORIENTED_EDGE ( 'NONE', *, *, #13669, .F. ) ;
#14389 = EDGE_CURVE ( 'NONE', #5700, #6405, #18044, .T. ) ;
#14390 = CARTESIAN_POINT ( 'NONE',  ( -41.00000000000000711, 53.00000000000000711, 13.50000000000000000 ) ) ;
#14391 = EDGE_LOOP ( 'NONE', ( #4681, #1547, #857, #13842 ) ) ;
#14392 = CARTESIAN_POINT ( 'NONE',  ( -0.9999999999999945599, -32.00000000000000000, 4.500000000000000888 ) ) ;
#14393 = VECTOR ( 'NONE', #9195, 1000.000000000000000 ) ;
#14394 = EDGE_LOOP ( 'NONE', ( #8817, #10144, #3305, #11696 ) ) ;
#14395 = DIRECTION ( 'NONE',  ( 0.000000000000000000, 1.000000000000000000, 0.000000000000000000 ) ) ;
#14396 = LINE ( 'NONE', #3913, #4361 ) ;
#14397 = CARTESIAN_POINT ( 'NONE',  ( 2.500000000000000000, 0.000000000000000000, 0.000000000000000000 ) ) ;
#14398 = AXIS2_PLACEMENT_3D ( 'NONE', #7760, #7956, #18549 ) ;
#14399 = CARTESIAN_POINT ( 'NONE',  ( 1.461580736456473684, 65.46158073645646880, 49.45000000109246940 ) ) ;
#14400 = DIRECTION ( 'NONE',  ( 1.000000000000000000, 0.000000000000000000, 0.000000000000000000 ) ) ;
#14401 = DIRECTION ( 'NONE',  ( 0.000000000000000000, 0.000000000000000000, -1.000000000000000000 ) ) ;
#14402 = VECTOR ( 'NONE', #17472, 1000.000000000000000 ) ;
#14403 = DIRECTION ( 'NONE',  ( 0.000000000000000000, 1.000000000000000000, 1.632680918566406793E-16 ) ) ;
#14404 = ORIENTED_EDGE ( 'NONE', *, *, #13726, .F. ) ;
#14405 = ORIENTED_EDGE ( 'NONE', *, *, #9166, .T. ) ;
#14406 = CARTESIAN_POINT ( 'NONE',  ( -11.64274437364854187, -30.14459132904234195, 1.201177507916956433 ) ) ;
#14407 = CARTESIAN_POINT ( 'NONE',  ( -14.99999999999999645, 3.000000000000000000, 20.99999999999998224 ) ) ;
#14408 = AXIS2_PLACEMENT_3D ( 'NONE', #15235, #4461, #10609 ) ;
#14409 = ORIENTED_EDGE ( 'NONE', *, *, #15657, .T. ) ;
#14410 = ADVANCED_FACE ( 'NONE', ( #80 ), #13691, .F. ) ;
#14411 = CARTESIAN_POINT ( 'NONE',  ( -12.48433729119799196, -22.35725562635139596, 1.861322492083043123 ) ) ;
#14412 = EDGE_CURVE ( 'NONE', #2559, #908, #4689, .T. ) ;
#14413 = VECTOR ( 'NONE', #12269, 1000.000000000000000 ) ;
#14414 = FACE_OUTER_BOUND ( 'NONE', #13093, .T. ) ;
#14415 = VERTEX_POINT ( 'NONE', #176 ) ;
#14416 = CARTESIAN_POINT ( 'NONE',  ( -15.63902057219073605, -27.04416526290807710, 35.33007249208304046 ) ) ;
#14417 = FACE_OUTER_BOUND ( 'NONE', #10279, .T. ) ;
#14418 = ORIENTED_EDGE ( 'NONE', *, *, #16188, .T. ) ;
#14419 = VECTOR ( 'NONE', #8512, 1000.000000000000000 ) ;
#14420 = CARTESIAN_POINT ( 'NONE',  ( -41.00000000000000711, 53.00000000000000711, -32.00000000000000000 ) ) ;
#14421 = PRODUCT_DEFINITION_SHAPE ( 'NONE', 'NONE',  #19408 ) ;
#14422 = ORIENTED_EDGE ( 'NONE', *, *, #19218, .F. ) ;
#14423 = LINE ( 'NONE', #2460, #3756 ) ;
#14424 = DIRECTION ( 'NONE',  ( -0.000000000000000000, 0.000000000000000000, -1.000000000000000000 ) ) ;
#14425 = DIRECTION ( 'NONE',  ( 1.000000000000000000, 0.000000000000000000, 0.000000000000000000 ) ) ;
#14426 = AXIS2_PLACEMENT_3D ( 'NONE', #15615, #8177, #6512 ) ;
#14427 = VECTOR ( 'NONE', #9177, 1000.000000000000000 ) ;
#14428 = CARTESIAN_POINT ( 'NONE',  ( -17.35725562635144215, -19.58745947852648683, 24.82617750791695954 ) ) ;
#14429 = FACE_BOUND ( 'NONE', #1247, .T. ) ;
#14430 = CARTESIAN_POINT ( 'NONE',  ( -45.00000000000000000, 0.000000000000000000, 54.99999999999998579 ) ) ;
#14431 = CARTESIAN_POINT ( 'NONE',  ( -19.41254052147348830, -26.35725562635142083, 7.763677507916958653 ) ) ;
#14432 = DIRECTION ( 'NONE',  ( 1.000000000000000000, 0.000000000000000000, 0.000000000000000000 ) ) ;
#14433 = EDGE_CURVE ( 'NONE', #2609, #5613, #16443, .T. ) ;
#14434 = EDGE_LOOP ( 'NONE', ( #9217, #14680, #468, #16320 ) ) ;
#14435 = CARTESIAN_POINT ( 'NONE',  ( -20.00369391078757886, -29.24501739517668142, 30.51757249208304401 ) ) ;
#14436 = VECTOR ( 'NONE', #8544, 1000.000000000000000 ) ;
#14437 = CARTESIAN_POINT ( 'NONE',  ( -11.46040770435012668, -27.78091578003887463, 37.73242750791694533 ) ) ;
#14438 = CARTESIAN_POINT ( 'NONE',  ( -2.066987300000001415, 63.14382582708705627, 48.00000000109246656 ) ) ;
#14439 = CARTESIAN_POINT ( 'NONE',  ( -17.35725562635140307, -28.41254052147349185, 35.54882249208304046 ) ) ;
#14440 = AXIS2_PLACEMENT_3D ( 'NONE', #9880, #1063, #17255 ) ;
#14441 = CARTESIAN_POINT ( 'NONE',  ( -2.066987300000001415, 64.00000000000000000, 44.75000000109247367 ) ) ;
#14442 = LINE ( 'NONE', #4159, #5021 ) ;
#14443 = CARTESIAN_POINT ( 'NONE',  ( -14.83517299489739649, -18.99999999999997868, 35.76367750791695954 ) ) ;
#14444 = DIRECTION ( 'NONE',  ( -0.000000000000000000, 0.000000000000000000, 1.000000000000000000 ) ) ;
#14445 = CARTESIAN_POINT ( 'NONE',  ( -16.17491895705301275, -18.95583473709189448, 35.54492750791695954 ) ) ;
#14446 = CARTESIAN_POINT ( 'NONE',  ( -1.485306817036799787, -35.50000000000000711, 8.000000000000007105 ) ) ;
#14447 = CARTESIAN_POINT ( 'NONE',  ( -20.04416526290809131, -22.82508104294700502, 41.89257249208303335 ) ) ;
#14448 = APPLICATION_CONTEXT ( 'automotive_design' ) ;
#14449 = CARTESIAN_POINT ( 'NONE',  ( 2.500000000000002220, 62.96446609406726935, 48.74999999999999289 ) ) ;
#14450 = CARTESIAN_POINT ( 'NONE',  ( -41.00000000000000711, 110.0000000000000000, 8.000000000000000000 ) ) ;
#14451 = VECTOR ( 'NONE', #13732, 1000.000000000000000 ) ;
#14452 = EDGE_CURVE ( 'NONE', #15669, #4696, #10970, .T. ) ;
#14453 = DIRECTION ( 'NONE',  ( 0.000000000000000000, 1.000000000000000000, 0.000000000000000000 ) ) ;
#14454 = CARTESIAN_POINT ( 'NONE',  ( -1.767766952966370209, 65.76776695296638309, 49.09999999999999432 ) ) ;
#14455 = CARTESIAN_POINT ( 'NONE',  ( -14.99999999999999645, 73.00000000000001421, 26.99999999999997868 ) ) ;
#14456 = VECTOR ( 'NONE', #13201, 1000.000000000000000 ) ;
#14457 = ORIENTED_EDGE ( 'NONE', *, *, #11807, .T. ) ;
#14458 =( NAMED_UNIT ( * ) SI_UNIT ( $, .STERADIAN. ) SOLID_ANGLE_UNIT ( ) );
#14459 = CARTESIAN_POINT ( 'NONE',  ( 2.066987300000001859, 63.14382582708704916, 46.70000000109248361 ) ) ;
#14460 = CARTESIAN_POINT ( 'NONE',  ( -11.46040770435012668, -27.78091578003887463, 6.232427507916956877 ) ) ;
#14461 = ADVANCED_FACE ( 'NONE', ( #12122 ), #8889, .F. ) ;
#14462 = DIRECTION ( 'NONE',  ( 2.602085213965211135E-16, -1.000000000000000000, 0.000000000000000000 ) ) ;
#14463 = CARTESIAN_POINT ( 'NONE',  ( -7.999999999999996447, -23.83517299489733432, 33.79882249208304046 ) ) ;
#14464 = CARTESIAN_POINT ( 'NONE',  ( -1.461580736456473462, 62.53841926354353120, 47.45000000109246230 ) ) ;
#14465 = ORIENTED_EDGE ( 'NONE', *, *, #9615, .T. ) ;
#14466 = FACE_OUTER_BOUND ( 'NONE', #16050, .T. ) ;
#14467 = CARTESIAN_POINT ( 'NONE',  ( -5.800000000000006928, 29.65425233947099315, 56.47747564417430510 ) ) ;
#14468 = CARTESIAN_POINT ( 'NONE',  ( 2.066987300000001415, 64.00000000000000000, 45.95000000109246940 ) ) ;
#14469 = FACE_OUTER_BOUND ( 'NONE', #16760, .T. ) ;
#14470 = CARTESIAN_POINT ( 'NONE',  ( -41.00000000000000711, 53.00000000000000711, 20.00000000000000000 ) ) ;
#14471 = CIRCLE ( 'NONE', #1965, 5.800000000000007816 ) ;
#14472 = FACE_OUTER_BOUND ( 'NONE', #18625, .T. ) ;
#14473 = CARTESIAN_POINT ( 'NONE',  ( 32.50000000000000000, 47.00000000000000711, -35.00000000000000000 ) ) ;
#14474 = ORIENTED_EDGE ( 'NONE', *, *, #9455, .F. ) ;
#14475 = ORIENTED_EDGE ( 'NONE', *, *, #3944, .F. ) ;
#14476 = CARTESIAN_POINT ( 'NONE',  ( -11.64274437364859693, -17.85540867095757989, 1.423822492083038904 ) ) ;
#14477 =( LENGTH_UNIT ( ) NAMED_UNIT ( * ) SI_UNIT ( .MILLI., .METRE. ) );
#14478 = VERTEX_POINT ( 'NONE', #11822 ) ;
#14480 = ORIENTED_EDGE ( 'NONE', *, *, #8179, .T. ) ;
#14479 = ORIENTED_EDGE ( 'NONE', *, *, #16094, .T. ) ;
#14481 = CARTESIAN_POINT ( 'NONE',  ( -17.95583473709191580, -23.03132541760400898, 8.419927507916959541 ) ) ;
#14482 = CARTESIAN_POINT ( 'NONE',  ( -8.855408670957631401, -20.64274437364852943, 36.63867750791695244 ) ) ;
#14483 = LINE ( 'NONE', #1054, #13839 ) ;
#14484 = CARTESIAN_POINT ( 'NONE',  ( -2.500000000000001776, 64.00000000000000000, 46.90000000218494591 ) ) ;
#14485 = DIRECTION ( 'NONE',  ( 1.000000000000000000, 0.000000000000000000, -0.000000000000000000 ) ) ;
#14486 = ORIENTED_EDGE ( 'NONE', *, *, #10536, .F. ) ;
#14487 = LINE ( 'NONE', #2255, #3164 ) ;
#14488 = ORIENTED_EDGE ( 'NONE', *, *, #16748, .F. ) ;
#14489 = CARTESIAN_POINT ( 'NONE',  ( -40.00000000000000000, 53.00000000000000711, 30.00000000000000000 ) ) ;
#14490 = ORIENTED_EDGE ( 'NONE', *, *, #12958, .T. ) ;
#14491 = LINE ( 'NONE', #14684, #11004 ) ;
#14492 = DIRECTION ( 'NONE',  ( 0.000000000000000000, -1.000000000000000000, -0.000000000000000000 ) ) ;
#14493 = DIRECTION ( 'NONE',  ( 0.000000000000000000, 0.000000000000000000, 1.000000000000000000 ) ) ;
#14494 = CARTESIAN_POINT ( 'NONE',  ( -1.265664690411616068E-16, 66.06698730000000808, 45.35000000109246798 ) ) ;
#14495 = DIRECTION ( 'NONE',  ( -1.000000000000000000, 0.000000000000000000, 0.000000000000000000 ) ) ;
#14496 = DIRECTION ( 'NONE',  ( 0.000000000000000000, 9.912705577010328508E-16, 1.000000000000000000 ) ) ;
#14497 = CARTESIAN_POINT ( 'NONE',  ( -25.00000000000000000, 110.0000000000000000, -37.50000000000000711 ) ) ;
#14498 = EDGE_LOOP ( 'NONE', ( #8041, #18413, #12995, #2851, #14776 ) ) ;
#14500 = ORIENTED_EDGE ( 'NONE', *, *, #9598, .F. ) ;
#14499 = ORIENTED_EDGE ( 'NONE', *, *, #14218, .F. ) ;
#14501 = EDGE_CURVE ( 'NONE', #7135, #4224, #1653, .T. ) ;
#14503 = ADVANCED_FACE ( 'NONE', ( #1451 ), #18220, .F. ) ;
#14502 = CARTESIAN_POINT ( 'NONE',  ( -11.46040770435012668, -27.78091578003887463, 37.73242750791694533 ) ) ;
#14504 = DIRECTION ( 'NONE',  ( -1.000000000000000000, -0.000000000000000000, -0.000000000000000000 ) ) ;
#14505 = ORIENTED_EDGE ( 'NONE', *, *, #16594, .F. ) ;
#14506 = CARTESIAN_POINT ( 'NONE',  ( -17.51566270880199738, -25.64274437364856496, 9.736322492083042235 ) ) ;
#14507 = EDGE_CURVE ( 'NONE', #14697, #11212, #504, .T. ) ;
#14508 = CARTESIAN_POINT ( 'NONE',  ( 1.035533905932739751, 61.50000000000000000, 45.45000000000000995 ) ) ;
#14509 = EDGE_LOOP ( 'NONE', ( #6935, #4920, #12033, #3907 ) ) ;
#14510 = CARTESIAN_POINT ( 'NONE',  ( -16.35725562635142794, -21.31951028609535470, 9.076177507916959541 ) ) ;
#14511 = EDGE_CURVE ( 'NONE', #6570, #1789, #267, .T. ) ;
#14512 = CARTESIAN_POINT ( 'NONE',  ( -1.767766952966370209, 65.76776695296638309, 49.09999999999999432 ) ) ;
#14513 = EDGE_LOOP ( 'NONE', ( #10579, #6742, #8400, #14614 ) ) ;
#14514 = DIRECTION ( 'NONE',  ( 0.000000000000000000, -1.000000000000000000, 0.000000000000000000 ) ) ;
#14515 = ORIENTED_EDGE ( 'NONE', *, *, #2222, .F. ) ;
#14516 = CYLINDRICAL_SURFACE ( 'NONE', #945, 2.999999999999999112 ) ;
#14517 = CARTESIAN_POINT ( 'NONE',  ( 0.000000000000000000, -6.000000000000000000, 0.000000000000000000 ) ) ;
#14518 = CARTESIAN_POINT ( 'NONE',  ( -2.500000000000011102, 62.96446609406727646, 47.75000000218493312 ) ) ;
#14519 = EDGE_CURVE ( 'NONE', #763, #5273, #4797, .T. ) ;
#14520 = CARTESIAN_POINT ( 'NONE',  ( -15.16482700510259640, -28.99999999999998224, 22.63867750791695954 ) ) ;
#14521 = AXIS2_PLACEMENT_3D ( 'NONE', #9727, #11970, #6008 ) ;
#14522 = CARTESIAN_POINT ( 'NONE',  ( -1.265664690411616068E-16, 66.06698730000000808, 47.15000000109247225 ) ) ;
#14523 = DIRECTION ( 'NONE',  ( -0.000000000000000000, 0.000000000000000000, 1.000000000000000000 ) ) ;
#14524 = CARTESIAN_POINT ( 'NONE',  ( -13.82508104294698192, -29.04416526290806644, 6.669927507916955989 ) ) ;
#14525 = FACE_OUTER_BOUND ( 'NONE', #8077, .T. ) ;
#14526 = ORIENTED_EDGE ( 'NONE', *, *, #13553, .T. ) ;
#14527 = ADVANCED_FACE ( 'NONE', ( #7324 ), #16541, .T. ) ;
#14528 = CARTESIAN_POINT ( 'NONE',  ( -13.49542703274174116, -28.95583473709188738, 8.642572492083040459 ) ) ;
#14529 = CARTESIAN_POINT ( 'NONE',  ( -16.17491895705301275, -18.95583473709189803, 40.79492750791695954 ) ) ;
#14530 = CARTESIAN_POINT ( 'NONE',  ( -0.8561741729129461742, 66.06698729999999387, 47.80000000109247082 ) ) ;
#14531 = CARTESIAN_POINT ( 'NONE',  ( -11.21908421996106320, -27.53959229564982181, 29.20507249208303335 ) ) ;
#14532 = MECHANICAL_DESIGN_GEOMETRIC_PRESENTATION_REPRESENTATION (  '', ( #17058 ), #19246 ) ;
#14533 = CARTESIAN_POINT ( 'NONE',  ( 4.592425496802577917E-16, 61.50000000000000000, 48.59999999999999432 ) ) ;
#14534 = EDGE_LOOP ( 'NONE', ( #1912, #7726, #5186, #8998 ) ) ;
#14535 = VECTOR ( 'NONE', #4778, 1000.000000000000000 ) ;
#14536 = CARTESIAN_POINT ( 'NONE',  ( 21.50000000000001421, 118.0000000000000142, 32.49999999999998579 ) ) ;
#14537 = CARTESIAN_POINT ( 'NONE',  ( -18.53959229564986799, -20.21908421996107563, 29.85742750791695599 ) ) ;
#14538 = DIRECTION ( 'NONE',  ( 0.000000000000000000, 0.000000000000000000, -1.000000000000000000 ) ) ;
#14539 = LINE ( 'NONE', #14839, #14097 ) ;
#14540 = LINE ( 'NONE', #1113, #11525 ) ;
#14541 = CARTESIAN_POINT ( 'NONE',  ( -19.24771351637086880, -26.64274437364857206, 41.23632249208304046 ) ) ;
#14542 = EDGE_CURVE ( 'NONE', #18278, #4488, #4396, .T. ) ;
#14543 = EDGE_CURVE ( 'NONE', #13439, #3909, #16784, .T. ) ;
#14544 = CARTESIAN_POINT ( 'NONE',  ( -1.530808498934192803E-16, 66.50000000000000000, 47.39999999999999858 ) ) ;
#14545 = CARTESIAN_POINT ( 'NONE',  ( -50.00000000000002132, 118.0000000000000142, 40.49999999999997868 ) ) ;
#14546 = DIRECTION ( 'NONE',  ( 0.000000000000000000, 0.000000000000000000, 1.000000000000000000 ) ) ;
#14547 = ADVANCED_FACE ( 'NONE', ( #16943 ), #9565, .F. ) ;
#14548 = CARTESIAN_POINT ( 'NONE',  ( -1.530808498934192803E-16, 66.50000000000000000, 48.99999999999999289 ) ) ;
#14549 = LINE ( 'NONE', #1418, #10830 ) ;
#14550 = PRESENTATION_LAYER_ASSIGNMENT (  '', '', ( #15815 ) ) ;
#14551 = AXIS2_PLACEMENT_3D ( 'NONE', #18117, #10356, #14975 ) ;
#14552 = VERTEX_POINT ( 'NONE', #12513 ) ;
#14553 = CARTESIAN_POINT ( 'NONE',  ( -14.83517299489739649, -18.99999999999997868, 4.263677507916958653 ) ) ;
#14554 = CARTESIAN_POINT ( 'NONE',  ( -11.46040770435012668, -27.78091578003887463, 0.9824275079169582092 ) ) ;
#14555 = PLANE ( 'NONE',  #703 ) ;
#14556 = CARTESIAN_POINT ( 'NONE',  ( -15.16482700510264436, -16.99999999999997868, 37.73632249208302625 ) ) ;
#14557 = CARTESIAN_POINT ( 'NONE',  ( 3.796994071234847710E-16, 61.93301269999999903, 48.35000000109246798 ) ) ;
#14558 = EDGE_CURVE ( 'NONE', #4945, #7898, #8112, .T. ) ;
#14559 = CARTESIAN_POINT ( 'NONE',  ( -17.51566270880201159, -22.35725562635141728, 29.63867750791695954 ) ) ;
#14560 = AXIS2_PLACEMENT_3D ( 'NONE', #6302, #1689, #16885 ) ;
#14561 = CARTESIAN_POINT ( 'NONE',  ( -17.35725562635144215, -19.58745947852648683, 9.076177507916957765 ) ) ;
#14562 = FACE_OUTER_BOUND ( 'NONE', #10865, .T. ) ;
#14563 = VECTOR ( 'NONE', #1733, 1000.000000000000000 ) ;
#14564 = CARTESIAN_POINT ( 'NONE',  ( 0.8561741729129460632, 66.06698730000000808, 47.70000000109248361 ) ) ;
#14565 = LINE ( 'NONE', #2321, #4335 ) ;
#14566 = CARTESIAN_POINT ( 'NONE',  ( 1.300000000000000044, 1.478016689125442484, -1.626303258728256651E-15 ) ) ;
#14567 = CARTESIAN_POINT ( 'NONE',  ( -1.265664690411616068E-16, 66.06698730000000808, 49.55000000109247082 ) ) ;
#14568 = DIRECTION ( 'NONE',  ( -1.000000000000000000, 0.000000000000000000, -2.081668171172167774E-16 ) ) ;
#14569 = DIRECTION ( 'NONE',  ( 0.000000000000000000, 0.000000000000000000, -1.000000000000000000 ) ) ;
#14570 = ORIENTED_EDGE ( 'NONE', *, *, #14027, .T. ) ;
#14571 = VERTEX_POINT ( 'NONE', #12321 ) ;
#14572 = PRODUCT_RELATED_PRODUCT_CATEGORY ( 'part', '', ( #1449 ) ) ;
#14573 = CARTESIAN_POINT ( 'NONE',  ( -21.95583473709189803, -26.04047135212049469, 9.955072492083038682 ) ) ;
#14574 = VECTOR ( 'NONE', #71, 1000.000000000000000 ) ;
#14575 = ORIENTED_EDGE ( 'NONE', *, *, #2432, .T. ) ;
#14576 = VECTOR ( 'NONE', #15043, 1000.000000000000000 ) ;
#14578 = ORIENTED_EDGE ( 'NONE', *, *, #16558, .F. ) ;
#14577 = VERTEX_POINT ( 'NONE', #15462 ) ;
#14579 = PRODUCT_DEFINITION_SHAPE ( 'NONE', 'NONE',  #19399 ) ;
#14580 = CARTESIAN_POINT ( 'NONE',  ( -11.95583473709190514, -24.63902057219072361, 39.26757249208304756 ) ) ;
#14581 = CARTESIAN_POINT ( 'NONE',  ( -16.71081734191527346, -16.95583473709190159, 35.54492750791695954 ) ) ;
#14582 = CARTESIAN_POINT ( 'NONE',  ( 1.300000000000000044, 1.108512516844082141, 0.6399999999999991251 ) ) ;
#14583 = CARTESIAN_POINT ( 'NONE',  ( -1.035533905932738641, 66.50000000000000000, 44.35000000218493454 ) ) ;
#14584 = DIRECTION ( 'NONE',  ( 1.000000000000000000, -0.000000000000000000, 0.000000000000000000 ) ) ;
#14585 = ADVANCED_FACE ( 'NONE', ( #12610 ), #6358, .T. ) ;
#14586 = VERTEX_POINT ( 'NONE', #3404 ) ;
#14587 = CARTESIAN_POINT ( 'NONE',  ( 2.499999999999996891, 62.96446609406726225, 47.14999999999999147 ) ) ;
#14588 = VERTEX_POINT ( 'NONE', #17128 ) ;
#14589 = CARTESIAN_POINT ( 'NONE',  ( -41.00000000000000711, 110.0000000000000000, 14.50000000000000000 ) ) ;
#14590 = VERTEX_POINT ( 'NONE', #13988 ) ;
#14591 = CARTESIAN_POINT ( 'NONE',  ( -1.262171526279624700, 62.35758450491420746, 45.00000000000000711 ) ) ;
#14592 = LINE ( 'NONE', #12921, #7484 ) ;
#14593 = CARTESIAN_POINT ( 'NONE',  ( -3.155775640247338920, -41.39960408384398249, 3.000000000000000000 ) ) ;
#14594 = VECTOR ( 'NONE', #17966, 1000.000000000000000 ) ;
#14595 = CARTESIAN_POINT ( 'NONE',  ( -2.066987300000001415, 64.00000000000000000, 44.75000000109247367 ) ) ;
#14596 = ADVANCED_BREP_SHAPE_REPRESENTATION ( '', ( #10129, #1791 ), #2636 ) ;
#14597 = VECTOR ( 'NONE', #8680, 1000.000000000000227 ) ;
#14598 = PLANE ( 'NONE',  #4086 ) ;
#14599 = CARTESIAN_POINT ( 'NONE',  ( -1.767766952966369765, 62.23223304703363112, 47.00000000218494733 ) ) ;
#14600 = CARTESIAN_POINT ( 'NONE',  ( -40.00000000000000000, 53.00000000000000711, 30.00000000000000000 ) ) ;
#14601 = EDGE_LOOP ( 'NONE', ( #1290, #9666, #4988, #15687 ) ) ;
#14603 = ORIENTED_EDGE ( 'NONE', *, *, #17950, .F. ) ;
#14602 = ORIENTED_EDGE ( 'NONE', *, *, #19355, .T. ) ;
#14604 = CARTESIAN_POINT ( 'NONE',  ( -18.78091578003889950, -27.53959229564985378, 39.04492750791695954 ) ) ;
#14605 = LINE ( 'NONE', #19023, #8053 ) ;
#14606 = ORIENTED_EDGE ( 'NONE', *, *, #3873, .F. ) ;
#14607 = CARTESIAN_POINT ( 'NONE',  ( -17.95583473709190869, -24.96867458239598037, 4.705072492083043123 ) ) ;
#14608 = VECTOR ( 'NONE', #16671, 1000.000000000000000 ) ;
#14609 = VECTOR ( 'NONE', #13381, 1000.000000000000000 ) ;
#14610 = CARTESIAN_POINT ( 'NONE',  ( 1.300000000000000044, 1.478016689125442484, -1.626303258728256651E-15 ) ) ;
#14611 = ORIENTED_EDGE ( 'NONE', *, *, #2292, .F. ) ;
#14612 = CARTESIAN_POINT ( 'NONE',  ( -16.64274437364858272, -21.48433729119797420, 42.54882249208304756 ) ) ;
#14613 = CARTESIAN_POINT ( 'NONE',  ( 1.035533905932738197, 66.50000000000000000, 48.94999999999999574 ) ) ;
#14614 = ORIENTED_EDGE ( 'NONE', *, *, #15828, .F. ) ;
#14615 = CARTESIAN_POINT ( 'NONE',  ( -25.00000000000000711, 110.0000000000000000, -25.50000000000000000 ) ) ;
#14616 = VERTEX_POINT ( 'NONE', #2030 ) ;
#14617 = DIRECTION ( 'NONE',  ( 5.782411586589357392E-17, 0.000000000000000000, 1.000000000000000000 ) ) ;
#14618 = CARTESIAN_POINT ( 'NONE',  ( -2.500000000000001776, 64.00000000000000000, 49.99999999999999289 ) ) ;
#14619 = DIRECTION ( 'NONE',  ( 0.000000000000000000, -1.000000000000000000, 0.000000000000000000 ) ) ;
#14620 = PRODUCT_CONTEXT ( 'NONE', #2679, 'mechanical' ) ;
#14621 = CARTESIAN_POINT ( 'NONE',  ( -2.500000000000001776, 64.00000000000000000, 48.39999999999999858 ) ) ;
#14622 = CARTESIAN_POINT ( 'NONE',  ( -17.64274437364855430, -28.24771351637087236, 28.32617750791695954 ) ) ;
#14623 = CARTESIAN_POINT ( 'NONE',  ( -8.528048594804062077, -45.28611686177728046, 3.000000000000000000 ) ) ;
#14625 = EDGE_CURVE ( 'NONE', #15781, #14815, #8021, .T. ) ;
#14624 = CARTESIAN_POINT ( 'NONE',  ( -20.04416526290808065, -25.17491895705300209, 2.732427507916957765 ) ) ;
#14626 = DIRECTION ( 'NONE',  ( -0.000000000000000000, -0.000000000000000000, -1.000000000000000000 ) ) ;
#14627 = ORIENTED_EDGE ( 'NONE', *, *, #15356, .F. ) ;
#14628 = CARTESIAN_POINT ( 'NONE',  ( -11.21908421996106320, -27.53959229564982181, 2.955072492083040903 ) ) ;
#14629 = CARTESIAN_POINT ( 'NONE',  ( -21.14459132904236327, -27.35725562635143149, 2.513677507916956433 ) ) ;
#14630 = DIRECTION ( 'NONE',  ( -0.000000000000000000, -0.000000000000000000, -1.000000000000000000 ) ) ;
#14631 = CARTESIAN_POINT ( 'NONE',  ( -17.64274437364858983, -19.75228648362910633, 42.54882249208304046 ) ) ;
#14632 = DIRECTION ( 'NONE',  ( 0.5773502691896176264, -0.8164965809277319186, 0.000000000000000000 ) ) ;
#14633 = ORIENTED_EDGE ( 'NONE', *, *, #18776, .F. ) ;
#14634 = CARTESIAN_POINT ( 'NONE',  ( -0.1250000000000104083, 32.14680374315353362, 54.33847763108504125 ) ) ;
#14635 = DIRECTION ( 'NONE',  ( -1.000000000000000000, -0.000000000000000000, -2.081668171172167774E-16 ) ) ;
#14636 = EDGE_CURVE ( 'NONE', #11634, #11674, #9475, .T. ) ;
#14637 = LINE ( 'NONE', #13055, #8913 ) ;
#14638 = CARTESIAN_POINT ( 'NONE',  ( -17.35725562635144215, -19.58745947852648683, 40.57617750791696665 ) ) ;
#14639 = CARTESIAN_POINT ( 'NONE',  ( -1.040834085586084257E-14, 29.74264068711925901, 56.74264068711929809 ) ) ;
#14640 = CARTESIAN_POINT ( 'NONE',  ( -15.16482700510263371, -18.99999999999997868, 37.73632249208303335 ) ) ;
#14641 = CARTESIAN_POINT ( 'NONE',  ( -1.035533905932738641, 66.50000000000000000, 46.64999999999999147 ) ) ;
#14642 = DIRECTION ( 'NONE',  ( 1.000000000000000000, -0.000000000000000000, -0.000000000000000000 ) ) ;
#14643 = DIRECTION ( 'NONE',  ( 0.000000000000000000, -1.000000000000000000, 0.000000000000000000 ) ) ;
#14644 = CARTESIAN_POINT ( 'NONE',  ( -2.500000000000001776, 64.00000000000000000, 47.59999999999999432 ) ) ;
#14645 = CARTESIAN_POINT ( 'NONE',  ( 4.160453206537118476, 26.88344170207930617, 59.60057016663805740 ) ) ;
#14646 = VERTEX_POINT ( 'NONE', #5262 ) ;
#14647 = EDGE_CURVE ( 'NONE', #13230, #13992, #6450, .T. ) ;
#14648 = CARTESIAN_POINT ( 'NONE',  ( -4.012830983233701687, 26.60336399182265055, 59.52836399182262994 ) ) ;
#14649 = EDGE_CURVE ( 'NONE', #12225, #4598, #2223, .T. ) ;
#14650 = CARTESIAN_POINT ( 'NONE',  ( -12.04416526290807887, -24.96867458239596260, 37.29492750791695954 ) ) ;
#14651 = DIRECTION ( 'NONE',  ( -7.709882115452476934E-17, -0.000000000000000000, -1.000000000000000000 ) ) ;
#14652 = EDGE_CURVE ( 'NONE', #18273, #3614, #9283, .T. ) ;
#14653 = CARTESIAN_POINT ( 'NONE',  ( -18.78091578003892081, -20.46040770435013556, 10.83007249208303691 ) ) ;
#14654 = CARTESIAN_POINT ( 'NONE',  ( -0.8561741729129461742, 66.06698729999999387, 48.80000000109247082 ) ) ;
#14655 = CARTESIAN_POINT ( 'NONE',  ( -12.31951028609537602, -22.64274437364854364, 36.63867750791695244 ) ) ;
#14656 = CARTESIAN_POINT ( 'NONE',  ( -16.50457296725820555, -28.95583473709189803, 1.857427507916957987 ) ) ;
#14657 = CARTESIAN_POINT ( 'NONE',  ( 0.000000000000000000, -1.178949249685214307, 2.042000000000002036 ) ) ;
#14658 = CARTESIAN_POINT ( 'NONE',  ( -0.1250000000000104083, 31.97002704785689531, 54.16170093578840294 ) ) ;
#14659 = PLANE ( 'NONE',  #4974 ) ;
#14660 = AXIS2_PLACEMENT_3D ( 'NONE', #2602, #9854, #4079 ) ;
#14661 = CARTESIAN_POINT ( 'NONE',  ( -41.00000000000000711, 53.00000000000000711, 26.50000000000000000 ) ) ;
#14662 = CARTESIAN_POINT ( 'NONE',  ( 1.461580736456473906, 62.53841926354353120, 49.25000000109246656 ) ) ;
#14663 = DIRECTION ( 'NONE',  ( 0.000000000000000000, 0.000000000000000000, -1.000000000000000000 ) ) ;
#14664 = CARTESIAN_POINT ( 'NONE',  ( 3.099999999999998757, 0.000000000000000000, 0.000000000000000000 ) ) ;
#14665 = ADVANCED_FACE ( 'NONE', ( #658 ), #18417, .T. ) ;
#14666 = ORIENTED_EDGE ( 'NONE', *, *, #5296, .T. ) ;
#14667 = EDGE_LOOP ( 'NONE', ( #11196, #4976, #11164, #9788 ) ) ;
#14668 = CARTESIAN_POINT ( 'NONE',  ( -11.35725562635139418, -29.97976432393972601, 8.423822492083040459 ) ) ;
#14669 = AXIS2_PLACEMENT_3D ( 'NONE', #17803, #2702, #4380 ) ;
#14670 = EDGE_LOOP ( 'NONE', ( #73, #19190 ) ) ;
#14671 = CARTESIAN_POINT ( 'NONE',  ( -9.955834737091903364, -25.17491895705295235, 2.517572492083040903 ) ) ;
#14673 = ORIENTED_EDGE ( 'NONE', *, *, #14452, .T. ) ;
#14672 = VERTEX_POINT ( 'NONE', #12419 ) ;
#14674 = CARTESIAN_POINT ( 'NONE',  ( -12.68318583509882380, -26.07549068051207541, 39.70507249208305467 ) ) ;
#14675 = CARTESIAN_POINT ( 'NONE',  ( -9.996306089212364299, -29.24501739517662813, 27.23242750791696309 ) ) ;
#14676 = CIRCLE ( 'NONE', #7806, 2.499999999999998668 ) ;
#14677 = DIRECTION ( 'NONE',  ( 0.000000000000000000, 0.000000000000000000, 1.000000000000000000 ) ) ;
#14678 = CARTESIAN_POINT ( 'NONE',  ( 2.066987300000001859, 64.85617417291294373, 49.20000000109247651 ) ) ;
#14679 = ORIENTED_EDGE ( 'NONE', *, *, #10487, .F. ) ;
#14680 = ORIENTED_EDGE ( 'NONE', *, *, #2928, .F. ) ;
#14681 = DIRECTION ( 'NONE',  ( -1.000000000000000000, 0.000000000000000000, -7.304098846218135653E-17 ) ) ;
#14682 = ORIENTED_EDGE ( 'NONE', *, *, #13937, .T. ) ;
#14683 = ORIENTED_EDGE ( 'NONE', *, *, #14649, .F. ) ;
#14684 = CARTESIAN_POINT ( 'NONE',  ( -25.00000000000000000, 53.00000000000000711, 20.00000000000000000 ) ) ;
#14685 = DIRECTION ( 'NONE',  ( 0.000000000000000000, -0.5000000000000009992, -0.8660254037844380415 ) ) ;
#14686 = CARTESIAN_POINT ( 'NONE',  ( -4.189607678530337331, 26.72836399182265055, 59.40336399182262284 ) ) ;
#14687 = VECTOR ( 'NONE', #18659, 1000.000000000000000 ) ;
#14688 = CARTESIAN_POINT ( 'NONE',  ( -2.066987300000001415, 64.00000000000000000, 48.95000000109246940 ) ) ;
#14689 = DIRECTION ( 'NONE',  ( -0.000000000000000000, -0.000000000000000000, 1.000000000000000000 ) ) ;
#14690 = VECTOR ( 'NONE', #7382, 1000.000000000000000 ) ;
#14691 = DIRECTION ( 'NONE',  ( 0.000000000000000000, 0.000000000000000000, 1.000000000000000000 ) ) ;
#14692 = VECTOR ( 'NONE', #3825, 1000.000000000000000 ) ;
#14693 = DIRECTION ( 'NONE',  ( 0.000000000000000000, 0.000000000000000000, -1.000000000000000000 ) ) ;
#14694 = EDGE_CURVE ( 'NONE', #9587, #7631, #18317, .T. ) ;
#14695 = ORIENTED_EDGE ( 'NONE', *, *, #16728, .T. ) ;
#14697 = VERTEX_POINT ( 'NONE', #17037 ) ;
#14696 = VERTEX_POINT ( 'NONE', #6729 ) ;
#14698 = CARTESIAN_POINT ( 'NONE',  ( -13.82508104294698192, -29.04416526290806644, 38.16992750791695244 ) ) ;
#14699 = CARTESIAN_POINT ( 'NONE',  ( 3.000000000000000888, 0.000000000000000000, 0.000000000000000000 ) ) ;
#14700 = ORIENTED_EDGE ( 'NONE', *, *, #1719, .T. ) ;
#14701 = VERTEX_POINT ( 'NONE', #18604 ) ;
#14702 = CARTESIAN_POINT ( 'NONE',  ( -19.41254052147350961, -21.64274437364857562, 42.11132249208304046 ) ) ;
#14703 = AXIS2_PLACEMENT_3D ( 'NONE', #14236, #11096, #2282 ) ;
#14704 = DIRECTION ( 'NONE',  ( -7.709882115452476934E-17, -0.000000000000000000, -1.000000000000000000 ) ) ;
#14705 = EDGE_CURVE ( 'NONE', #7257, #13043, #3594, .T. ) ;
#14706 = VERTEX_POINT ( 'NONE', #6645 ) ;
#14707 = CARTESIAN_POINT ( 'NONE',  ( -11.99999999999999289, -24.16482700510258752, 5.576177507916960430 ) ) ;
#14708 = AXIS2_PLACEMENT_3D ( 'NONE', #19326, #5704, #10186 ) ;
#14709 = DIRECTION ( 'NONE',  ( 0.000000000000000000, 0.000000000000000000, -1.000000000000000000 ) ) ;
#14710 = VERTEX_POINT ( 'NONE', #16842 ) ;
#14711 = PLANE ( 'NONE',  #3760 ) ;
#14712 = ORIENTED_EDGE ( 'NONE', *, *, #6309, .T. ) ;
#14713 = CARTESIAN_POINT ( 'NONE',  ( -40.00000000000000711, 110.0000000000000000, 26.50000000000000000 ) ) ;
#14714 = DIRECTION ( 'NONE',  ( -1.000000000000000000, 0.000000000000000000, 0.000000000000000000 ) ) ;
#14715 = DIRECTION ( 'NONE',  ( -1.000000000000000000, -0.000000000000000000, -0.000000000000000000 ) ) ;
#14716 = VECTOR ( 'NONE', #13822, 1000.000000000000000 ) ;
#14717 = APPLICATION_PROTOCOL_DEFINITION ( 'draft international standard', 'automotive_design', 1998, #7436 ) ;
#14718 = CARTESIAN_POINT ( 'NONE',  ( 50.00000000000000000, 0.000000000000000000, -60.00000000000000000 ) ) ;
#14719 = CARTESIAN_POINT ( 'NONE',  ( -12.35725562635143682, -19.75228648362908501, 20.45117750791695954 ) ) ;
#14720 = AXIS2_PLACEMENT_3D ( 'NONE', #12553, #12645, #15593 ) ;
#14721 = CARTESIAN_POINT ( 'NONE',  ( -50.00000000000002132, 118.0000000000000142, -60.00000000000002132 ) ) ;
#14722 = ADVANCED_FACE ( 'NONE', ( #9661 ), #11130, .F. ) ;
#14723 = CARTESIAN_POINT ( 'NONE',  ( -20.04416526290808065, -25.17491895705300209, 7.982427507916958653 ) ) ;
#14724 = VECTOR ( 'NONE', #3548, 1000.000000000000000 ) ;
#14725 = CARTESIAN_POINT ( 'NONE',  ( -37.50000000000002132, -6.000000000000000000, -25.00000000000002132 ) ) ;
#14726 = EDGE_LOOP ( 'NONE', ( #8320, #13609, #9990, #6469 ) ) ;
#14727 = CARTESIAN_POINT ( 'NONE',  ( -11.46040770435014977, -20.21908421996103655, 1.642572492083041125 ) ) ;
#14728 = CARTESIAN_POINT ( 'NONE',  ( -8.855408670957631401, -20.64274437364852943, 10.38867750791695599 ) ) ;
#14729 = VECTOR ( 'NONE', #13249, 1000.000000000000000 ) ;
#14730 = CARTESIAN_POINT ( 'NONE',  ( 2.066987300000001415, 64.00000000000000000, 45.95000000109246940 ) ) ;
#14731 = CARTESIAN_POINT ( 'NONE',  ( -11.95583473709190514, -24.63902057219072361, 2.517572492083043123 ) ) ;
#14732 = CYLINDRICAL_SURFACE ( 'NONE', #16616, 4.250000000000000000 ) ;
#14733 = ORIENTED_EDGE ( 'NONE', *, *, #3878, .F. ) ;
#14734 = VECTOR ( 'NONE', #19228, 1000.000000000000000 ) ;
#14735 = CARTESIAN_POINT ( 'NONE',  ( -40.00000000000000000, 53.00000000000000711, 30.00000000000000000 ) ) ;
#14736 = CARTESIAN_POINT ( 'NONE',  ( -15.16482700510259640, -28.99999999999998224, 38.38867750791695954 ) ) ;
#14737 = DIRECTION ( 'NONE',  ( -1.000000000000000000, 0.000000000000000000, 0.000000000000000000 ) ) ;
#14738 = DIRECTION ( 'NONE',  ( -0.7071067811865561215, -0.4999999999999953926, 0.4999999999999925060 ) ) ;
#14739 = CIRCLE ( 'NONE', #17250, 0.2000000000000000944 ) ;
#14740 = DIRECTION ( 'NONE',  ( -1.000000000000000000, 0.000000000000000000, -0.000000000000000000 ) ) ;
#14741 = CARTESIAN_POINT ( 'NONE',  ( -19.95583473709190514, -25.50457296725823042, 36.20507249208304046 ) ) ;
#14742 = CARTESIAN_POINT ( 'NONE',  ( 1.767766952966369987, 65.76776695296638309, 47.29999999999999716 ) ) ;
#14743 = CARTESIAN_POINT ( 'NONE',  ( 3.796994071234847710E-16, 61.93301269999999903, 48.35000000109246798 ) ) ;
#14744 = VECTOR ( 'NONE', #11852, 1000.000000000000000 ) ;
#14745 = PRODUCT_DEFINITION_SHAPE ( 'NONE', 'NONE',  #4165 ) ;
#14746 = CARTESIAN_POINT ( 'NONE',  ( -41.00000000000000711, 110.0000000000000000, -44.00000000000000000 ) ) ;
#14747 = CARTESIAN_POINT ( 'NONE',  ( -2.500000000000001776, 64.00000000000000000, 45.19999999999999574 ) ) ;
#14748 = CARTESIAN_POINT ( 'NONE',  ( 44.99999999999998579, 0.000000000000000000, -53.39999999999999147 ) ) ;
#14749 = AXIS2_PLACEMENT_3D ( 'NONE', #3563, #808, #13952 ) ;
#14750 = VERTEX_POINT ( 'NONE', #13790 ) ;
#14751 = EDGE_CURVE ( 'NONE', #18739, #3513, #370, .T. ) ;
#14752 = EDGE_CURVE ( 'NONE', #7844, #6260, #13888, .T. ) ;
#14753 = VECTOR ( 'NONE', #2623, 1000.000000000000000 ) ;
#14754 = CARTESIAN_POINT ( 'NONE',  ( -10.58745947852649927, -21.64274437364853654, -0.1113224920830418047 ) ) ;
#14755 = CARTESIAN_POINT ( 'NONE',  ( -9.955834737091912245, -22.82508104294696594, 15.85742750791695777 ) ) ;
#14756 = CARTESIAN_POINT ( 'NONE',  ( -1.767766952966370209, 65.76776695296638309, 47.60000000218494165 ) ) ;
#14757 = EDGE_CURVE ( 'NONE', #16538, #297, #1252, .T. ) ;
#14758 = CARTESIAN_POINT ( 'NONE',  ( -15.16482700510264436, -16.99999999999997868, 42.98632249208304756 ) ) ;
#14759 = AXIS2_PLACEMENT_3D ( 'NONE', #5268, #2701, #11506 ) ;
#14760 = CARTESIAN_POINT ( 'NONE',  ( -1.265664690411616068E-16, 66.06698730000000808, 48.75000000109246656 ) ) ;
#14761 = CARTESIAN_POINT ( 'NONE',  ( -10.75228648362910100, -26.64274437364854009, 6.013677507916958653 ) ) ;
#14762 = CARTESIAN_POINT ( 'NONE',  ( -20.04416526290808065, -25.17491895705300209, 2.732427507916958209 ) ) ;
#14763 = FACE_OUTER_BOUND ( 'NONE', #1958, .T. ) ;
#14764 = CIRCLE ( 'NONE', #1623, 2.649999999999999467 ) ;
#14765 = LINE ( 'NONE', #6046, #6234 ) ;
#14766 = CARTESIAN_POINT ( 'NONE',  ( 0.000000000000000000, 0.000000000000000000, 30.00000000000000000 ) ) ;
#14767 = VECTOR ( 'NONE', #11062, 1000.000000000000000 ) ;
#14768 = FACE_OUTER_BOUND ( 'NONE', #8535, .T. ) ;
#14769 = EDGE_CURVE ( 'NONE', #12144, #17252, #6857, .T. ) ;
#14770 = CARTESIAN_POINT ( 'NONE',  ( -1.461580736456473462, 62.53841926354353120, 45.05000000109246372 ) ) ;
#14771 = CARTESIAN_POINT ( 'NONE',  ( -1.040834085586084257E-14, 25.64142135623728080, 60.84386001800126564 ) ) ;
#14772 = EDGE_CURVE ( 'NONE', #18998, #1273, #19208, .T. ) ;
#14773 = ADVANCED_FACE ( 'NONE', ( #5776 ), #16165, .F. ) ;
#14774 = DIRECTION ( 'NONE',  ( 0.000000000000000000, 0.4999999999999991118, -0.8660254037844391517 ) ) ;
#14775 = VERTEX_POINT ( 'NONE', #3830 ) ;
#14776 = ORIENTED_EDGE ( 'NONE', *, *, #641, .T. ) ;
#14777 = CARTESIAN_POINT ( 'NONE',  ( -11.35725562635139418, -29.97976432393972601, 18.92382249208303691 ) ) ;
#14778 = PRESENTATION_STYLE_ASSIGNMENT (( #19090 ) ) ;
#14779 = DIRECTION ( 'NONE',  ( 1.000000000000000000, 0.000000000000000000, -0.000000000000000000 ) ) ;
#14781 = VERTEX_POINT ( 'NONE', #8426 ) ;
#14780 = ORIENTED_EDGE ( 'NONE', *, *, #5139, .T. ) ;
#14782 = CARTESIAN_POINT ( 'NONE',  ( -12.48433729119798130, -25.64274437364855075, 0.7636775079169598746 ) ) ;
#14783 = DIRECTION ( 'NONE',  ( -0.000000000000000000, -0.000000000000000000, -1.000000000000000000 ) ) ;
#14784 = CARTESIAN_POINT ( 'NONE',  ( -20.97976432393977575, -20.35725562635143504, 40.13867750791695954 ) ) ;
#14785 = AXIS2_PLACEMENT_3D ( 'NONE', #15539, #2110, #7797 ) ;
#14786 = DIRECTION ( 'NONE',  ( 1.000000000000000000, 0.000000000000000000, -0.000000000000000000 ) ) ;
#14787 = CARTESIAN_POINT ( 'NONE',  ( -1.461580736456473906, 65.46158073645646880, 49.45000000109246940 ) ) ;
#14788 = ORIENTED_EDGE ( 'NONE', *, *, #11868, .F. ) ;
#14789 = ORIENTED_EDGE ( 'NONE', *, *, #18004, .F. ) ;
#14790 = CARTESIAN_POINT ( 'NONE',  ( 1.767766952966370653, 62.23223304703363112, 47.09999999999999432 ) ) ;
#14791 = DIRECTION ( 'NONE',  ( 0.000000000000000000, 1.000000000000000000, 0.000000000000000000 ) ) ;
#14792 = ORIENTED_EDGE ( 'NONE', *, *, #14507, .F. ) ;
#14793 = FACE_BOUND ( 'NONE', #11521, .T. ) ;
#14794 = CARTESIAN_POINT ( 'NONE',  ( -11.05206702929440254, -21.80946413714601562, 1.107186296610940179E-15 ) ) ;
#14795 = CARTESIAN_POINT ( 'NONE',  ( 43.50000000000001421, 2.999000000000001442, 32.49999999999998579 ) ) ;
#14796 = CARTESIAN_POINT ( 'NONE',  ( 0.8561741729129460632, 66.06698729999999387, 47.90000000109247225 ) ) ;
#14797 = ADVANCED_FACE ( 'NONE', ( #12925 ), #9568, .T. ) ;
#14798 = EDGE_CURVE ( 'NONE', #12337, #7234, #15881, .T. ) ;
#14799 = PLANE ( 'NONE',  #16624 ) ;
#14800 = CARTESIAN_POINT ( 'NONE',  ( 43.49999999999997868, 118.0000000000000142, -52.50000000000002132 ) ) ;
#14801 = ORIENTED_EDGE ( 'NONE', *, *, #5411, .T. ) ;
#14803 = ORIENTED_EDGE ( 'NONE', *, *, #12757, .F. ) ;
#14802 = ORIENTED_EDGE ( 'NONE', *, *, #13095, .T. ) ;
#14804 = EDGE_CURVE ( 'NONE', #8146, #628, #1433, .T. ) ;
#14805 = CARTESIAN_POINT ( 'NONE',  ( -18.64274437364853654, -29.97976432393976509, 2.076177507916956433 ) ) ;
#14806 = CARTESIAN_POINT ( 'NONE',  ( 3.999999999999998224, 67.00000000000000000, 30.00000000000000000 ) ) ;
#14807 = ORIENTED_EDGE ( 'NONE', *, *, #1003, .T. ) ;
#14808 = ORIENTED_EDGE ( 'NONE', *, *, #13475, .T. ) ;
#14809 = CARTESIAN_POINT ( 'NONE',  ( -12.92450931948790149, -21.68318583509881137, 1.642572492083043123 ) ) ;
#14810 = DIRECTION ( 'NONE',  ( 1.000000000000000000, 0.000000000000000000, 0.000000000000000000 ) ) ;
#14811 = CARTESIAN_POINT ( 'NONE',  ( -10.00000000000000000, -16.78846153846157918, -16.05769230769231015 ) ) ;
#14812 = ORIENTED_EDGE ( 'NONE', *, *, #757, .T. ) ;
#14813 = CARTESIAN_POINT ( 'NONE',  ( -12.04416526290807887, -24.96867458239596260, 5.794927507916960430 ) ) ;
#14814 = CARTESIAN_POINT ( 'NONE',  ( -15.00000000000001421, -18.99999999999997868, -4.336808689942017736E-16 ) ) ;
#14815 = VERTEX_POINT ( 'NONE', #4211 ) ;
#14816 = LINE ( 'NONE', #4630, #10627 ) ;
#14817 = ORIENTED_EDGE ( 'NONE', *, *, #988, .F. ) ;
#14818 = EDGE_CURVE ( 'NONE', #3100, #19316, #2734, .T. ) ;
#14819 = DIRECTION ( 'NONE',  ( 0.000000000000000000, -1.000000000000000000, 0.000000000000000000 ) ) ;
#14820 = DIRECTION ( 'NONE',  ( 0.7071067811865414665, -0.5000000000000057732, 0.5000000000000028866 ) ) ;
#14821 = CARTESIAN_POINT ( 'NONE',  ( -41.00000000000000711, 53.00000000000000711, -18.00000000000000000 ) ) ;
#14822 = SHAPE_DEFINITION_REPRESENTATION ( #17890, #9996 ) ;
#14823 = CARTESIAN_POINT ( 'NONE',  ( -4.101219330881938241, 32.64264068711930378, 53.84264068711927109 ) ) ;
#14824 = CARTESIAN_POINT ( 'NONE',  ( -4.999999999999996447, -32.00000000000000000, 9.500000000000001776 ) ) ;
#14825 =( NAMED_UNIT ( * ) PLANE_ANGLE_UNIT ( ) SI_UNIT ( $, .RADIAN. ) );
#14826 = CARTESIAN_POINT ( 'NONE',  ( -9.955834737091912245, -22.82508104294696594, 5.357427507916956877 ) ) ;
#14827 = DIRECTION ( 'NONE',  ( -0.5000000000000034417, 1.060575238724904696E-16, -0.8660254037844367092 ) ) ;
#14828 = ORIENTED_EDGE ( 'NONE', *, *, #3273, .T. ) ;
#14829 = CARTESIAN_POINT ( 'NONE',  ( -17.04047135212050890, -17.04416526290807710, 42.76757249208304046 ) ) ;
#14830 = CARTESIAN_POINT ( 'NONE',  ( -21.95583473709191580, -21.95952864787954084, 3.169927507916957321 ) ) ;
#14831 = CARTESIAN_POINT ( 'NONE',  ( 2.500000000000010658, 62.96446609406726225, 48.05000000218495160 ) ) ;
#14832 = CARTESIAN_POINT ( 'NONE',  ( -14.83517299489736985, -26.99999999999998579, 8.861322492083040459 ) ) ;
#14833 = CARTESIAN_POINT ( 'NONE',  ( -32.50000000000002132, -6.000000000000000000, -25.00000000000002132 ) ) ;
#14834 = ORIENTED_EDGE ( 'NONE', *, *, #18058, .T. ) ;
#14835 = CARTESIAN_POINT ( 'NONE',  ( -13.51548992270003957, -18.19996206762383650, -8.139499971887964371E-17 ) ) ;
#14836 = ORIENTED_EDGE ( 'NONE', *, *, #17506, .F. ) ;
#14837 = CARTESIAN_POINT ( 'NONE',  ( 0.000000000000000000, 64.00000000000000000, 49.99999999999999289 ) ) ;
#14838 = LINE ( 'NONE', #2969, #13934 ) ;
#14839 = CARTESIAN_POINT ( 'NONE',  ( -4.999999999999980460, 60.00000000000000711, 69.99999999999998579 ) ) ;
#14840 = CARTESIAN_POINT ( 'NONE',  ( 0.1499999999999973577, 0.000000000000000000, 2.600000000000000089 ) ) ;
#14841 = PLANE ( 'NONE',  #18811 ) ;
#14842 = CARTESIAN_POINT ( 'NONE',  ( -2.500000000000000888, 62.96446609406726935, 46.84999999999998721 ) ) ;
#14843 = CARTESIAN_POINT ( 'NONE',  ( -1.461580736456473462, 62.53841926354353120, 48.25000000109246656 ) ) ;
#14844 = DIRECTION ( 'NONE',  ( -1.000000000000000000, 0.000000000000000000, -1.541976423090495633E-16 ) ) ;
#14845 = CARTESIAN_POINT ( 'NONE',  ( 2.500000000000001776, 65.03553390593273775, 46.45000000000000284 ) ) ;
#14846 = DIRECTION ( 'NONE',  ( 1.000000000000000000, 0.000000000000000000, 0.000000000000000000 ) ) ;
#14847 = VERTEX_POINT ( 'NONE', #5487 ) ;
#14848 =( LENGTH_UNIT ( ) NAMED_UNIT ( * ) SI_UNIT ( .MILLI., .METRE. ) );
#14849 = CARTESIAN_POINT ( 'NONE',  ( -19.41254052147348830, -26.35725562635142083, 2.513677507916958209 ) ) ;
#14850 = STYLED_ITEM ( 'NONE', ( #5422 ), #17097 ) ;
#14851 = CARTESIAN_POINT ( 'NONE',  ( -19.24771351637089367, -21.35725562635142438, 19.13867750791695954 ) ) ;
#14852 = CARTESIAN_POINT ( 'NONE',  ( -2.500000000000001776, 64.00000000000000000, 47.70000000218494307 ) ) ;
#14853 = CARTESIAN_POINT ( 'NONE',  ( -10.58745947852648328, -26.35725562635138530, 2.736322492083041347 ) ) ;
#14854 = CARTESIAN_POINT ( 'NONE',  ( -1.461580736456473906, 65.46158073645646880, 46.45000000109246940 ) ) ;
#14855 = CARTESIAN_POINT ( 'NONE',  ( -10.58745947852649927, -21.64274437364853654, 5.138677507916957765 ) ) ;
#14856 = CARTESIAN_POINT ( 'NONE',  ( -10.58745947852649927, -21.64274437364853654, 5.138677507916957765 ) ) ;
#14857 = LINE ( 'NONE', #10532, #2237 ) ;
#14858 = CARTESIAN_POINT ( 'NONE',  ( -41.00000000000000711, 53.00000000000000711, -11.50000000000000000 ) ) ;
#14859 = LINE ( 'NONE', #11809, #11828 ) ;
#14860 = EDGE_CURVE ( 'NONE', #18337, #8383, #16030, .T. ) ;
#14861 = EDGE_CURVE ( 'NONE', #10054, #11529, #15789, .T. ) ;
#14862 = FACE_OUTER_BOUND ( 'NONE', #8317, .T. ) ;
#14863 = VECTOR ( 'NONE', #6628, 1000.000000000000000 ) ;
#14864 = CARTESIAN_POINT ( 'NONE',  ( -2.066987300000000971, 63.14382582708704916, 46.60000000109246798 ) ) ;
#14865 = CARTESIAN_POINT ( 'NONE',  ( -2.283493650000001818, 64.00000000000000000, 49.87500000054622973 ) ) ;
#14866 = ADVANCED_FACE ( 'NONE', ( #2540 ), #17538, .F. ) ;
#14867 = DIRECTION ( 'NONE',  ( 1.000000000000000000, 0.000000000000000000, 0.000000000000000000 ) ) ;
#14868 = ORIENTED_EDGE ( 'NONE', *, *, #12621, .F. ) ;
#14869 = ORIENTED_EDGE ( 'NONE', *, *, #8435, .F. ) ;
#14870 = CARTESIAN_POINT ( 'NONE',  ( -12.95952864787948755, -30.95583473709188382, 24.39257249208303691 ) ) ;
#14871 = EDGE_CURVE ( 'NONE', #9436, #3842, #11542, .T. ) ;
#14872 = SURFACE_SIDE_STYLE ('',( #8884 ) ) ;
#14873 = DIRECTION ( 'NONE',  ( 1.000000000000000000, 0.000000000000000000, 0.000000000000000000 ) ) ;
#14875 = VERTEX_POINT ( 'NONE', #17635 ) ;
#14874 = ORIENTED_EDGE ( 'NONE', *, *, #11885, .F. ) ;
#14876 = CARTESIAN_POINT ( 'NONE',  ( -14.36097942780923731, -27.04416526290806999, 17.16992750791696309 ) ) ;
#14877 = DIRECTION ( 'NONE',  ( -1.000000000000000000, 0.000000000000000000, 0.000000000000000000 ) ) ;
#14878 = CARTESIAN_POINT ( 'NONE',  ( -15.16482700510264436, -16.99999999999997868, 0.9863224920830391262 ) ) ;
#14879 = VECTOR ( 'NONE', #2094, 1000.000000000000000 ) ;
#14880 = VECTOR ( 'NONE', #16582, 1000.000000000000000 ) ;
#14881 = CARTESIAN_POINT ( 'NONE',  ( -2.066987300000001415, 63.14382582708705627, 48.80000000109247082 ) ) ;
#14882 = CARTESIAN_POINT ( 'NONE',  ( 2.066987300000001859, 64.85617417291294373, 48.40000000109247225 ) ) ;
#14883 = ORIENTED_EDGE ( 'NONE', *, *, #12825, .T. ) ;
#14884 = EDGE_LOOP ( 'NONE', ( #14013, #11820, #13250, #17131 ) ) ;
#14885 =( BOUNDED_CURVE ( )  B_SPLINE_CURVE ( 2, ( #849, #15664, #4082, #2235, #5372, #11615, #2412, #2508, #9855 ),
 .UNSPECIFIED., .F., .F. ) 
 B_SPLINE_CURVE_WITH_KNOTS ( ( 3, 2, 2, 2, 3 ),
 ( 0.3571428571428572618, 0.3750000000000000555, 0.3928571428571429047, 0.4107142857142856984, 0.4285714285714284921 ),
 .UNSPECIFIED. ) 
 CURVE ( )  GEOMETRIC_REPRESENTATION_ITEM ( )  RATIONAL_B_SPLINE_CURVE ( ( 0.9999999999999995559, 0.9238795325112871826, 1.000000000000000000, 0.9238795325112867385, 1.000000000000000000, 0.9238795325112867385, 1.000000000000000000, 0.9238795325112869605, 0.9999999999999997780 ) ) 
 REPRESENTATION_ITEM ( '' )  );
#14886 = DIRECTION ( 'NONE',  ( -1.000000000000000000, 0.000000000000000000, -0.000000000000000000 ) ) ;
#14887 = DIRECTION ( 'NONE',  ( 0.000000000000000000, 0.000000000000000000, 1.000000000000000000 ) ) ;
#14888 = ORIENTED_EDGE ( 'NONE', *, *, #13726, .T. ) ;
#14889 = LINE ( 'NONE', #12035, #13760 ) ;
#14890 = ADVANCED_FACE ( 'NONE', ( #10164 ), #8339, .F. ) ;
#14891 = CARTESIAN_POINT ( 'NONE',  ( -1.461580736456473462, 62.53841926354353120, 48.25000000109246656 ) ) ;
#14892 = DIRECTION ( 'NONE',  ( -1.000000000000000000, 0.000000000000000000, -0.000000000000000000 ) ) ;
#14893 = VECTOR ( 'NONE', #19017, 1000.000000000000000 ) ;
#14894 = AXIS2_PLACEMENT_3D ( 'NONE', #8523, #2356, #14312 ) ;
#14895 = CARTESIAN_POINT ( 'NONE',  ( -24.00000000000000711, 110.0000000000000000, -5.000000000000000888 ) ) ;
#14896 = EDGE_LOOP ( 'NONE', ( #15623, #16777, #8530 ) ) ;
#14898 = EDGE_LOOP ( 'NONE', ( #14007, #5087, #12993, #12816 ) ) ;
#14897 = ORIENTED_EDGE ( 'NONE', *, *, #2994, .T. ) ;
#14899 = CARTESIAN_POINT ( 'NONE',  ( -9.996306089212364299, -29.24501739517662813, 21.98242750791695599 ) ) ;
#14900 = CARTESIAN_POINT ( 'NONE',  ( 32.50000000000000000, 47.00000000000000711, -32.50000000000000000 ) ) ;
#14901 = EDGE_LOOP ( 'NONE', ( #13389, #16693, #492, #10708, #6276, #10154, #4204, #15745 ) ) ;
#14902 = VERTEX_POINT ( 'NONE', #15067 ) ;
#14903 = CARTESIAN_POINT ( 'NONE',  ( -11.99999999999999289, -23.83517299489735564, 23.29882249208304046 ) ) ;
#14904 = EDGE_CURVE ( 'NONE', #13602, #209, #15454, .T. ) ;
#14905 = EDGE_CURVE ( 'NONE', #1350, #7469, #10540, .T. ) ;
#14906 = CARTESIAN_POINT ( 'NONE',  ( 2.492551403682558675, 28.10514068711924196, 58.38014068711930804 ) ) ;
#14907 = CARTESIAN_POINT ( 'NONE',  ( -0.1250000000000104083, 33.66708332270461312, 52.46464466094069934 ) ) ;
#14908 = ORIENTED_EDGE ( 'NONE', *, *, #3846, .T. ) ;
#14909 = ADVANCED_FACE ( 'NONE', ( #10738 ), #1101, .T. ) ;
#14910 = CARTESIAN_POINT ( 'NONE',  ( -17.99999999999999645, -23.83517299489736985, 8.201177507916959541 ) ) ;
#14911 = VECTOR ( 'NONE', #5375, 1000.000000000000000 ) ;
#14912 = LINE ( 'NONE', #18347, #11293 ) ;
#14913 = ORIENTED_EDGE ( 'NONE', *, *, #9591, .F. ) ;
#14914 = VECTOR ( 'NONE', #2883, 1000.000000000000114 ) ;
#14915 = PLANE ( 'NONE',  #6269 ) ;
#14916 = PRODUCT_DEFINITION_SHAPE ( 'NONE', 'NONE',  #19395 ) ;
#14917 = EDGE_LOOP ( 'NONE', ( #7775, #7845, #12285, #12242 ) ) ;
#14918 = LINE ( 'NONE', #1490, #6612 ) ;
#14919 = CARTESIAN_POINT ( 'NONE',  ( -12.50000000000000000, -35.50000000000000000, 5.500000000000000000 ) ) ;
#14920 = CARTESIAN_POINT ( 'NONE',  ( 2.500000000000001776, 64.00000000000000000, 45.70000000218494307 ) ) ;
#14921 = SHAPE_DEFINITION_REPRESENTATION ( #19290, #12005 ) ;
#14922 = DIRECTION ( 'NONE',  ( -1.000000000000000000, -0.000000000000000000, -0.000000000000000000 ) ) ;
#14923 = CARTESIAN_POINT ( 'NONE',  ( -18.78091578003889950, -27.53959229564985378, 39.04492750791695954 ) ) ;
#14924 = CARTESIAN_POINT ( 'NONE',  ( -0.9999999999999945599, -32.00000000000000000, 9.500000000000001776 ) ) ;
#14925 = CARTESIAN_POINT ( 'NONE',  ( -15.16482700510259640, -28.99999999999998224, 12.13867750791695777 ) ) ;
#14926 = AXIS2_PLACEMENT_3D ( 'NONE', #18168, #4743, #10700 ) ;
#14927 = CARTESIAN_POINT ( 'NONE',  ( -25.00000000000000000, 53.00000000000000711, 30.00000000000000000 ) ) ;
#14928 = EDGE_LOOP ( 'NONE', ( #19024, #11561, #8986, #1753 ) ) ;
#14929 = VECTOR ( 'NONE', #8065, 1000.000000000000114 ) ;
#14930 = ADVANCED_FACE ( 'NONE', ( #7917 ), #260, .T. ) ;
#14931 = CARTESIAN_POINT ( 'NONE',  ( -9.955834737091903364, -25.17491895705294880, 7.767572492083041347 ) ) ;
#14932 = EDGE_CURVE ( 'NONE', #4327, #14325, #13782, .T. ) ;
#14933 = CARTESIAN_POINT ( 'NONE',  ( 2.066987300000001415, 64.00000000000000000, 45.15000000109247225 ) ) ;
#14934 = CARTESIAN_POINT ( 'NONE',  ( -17.07549068051208963, -26.31681416490115311, 9.517572492083044011 ) ) ;
#14935 = CARTESIAN_POINT ( 'NONE',  ( 1.753982408753060440, -43.60761626555502346, 3.000000000000000000 ) ) ;
#14936 = ORIENTED_EDGE ( 'NONE', *, *, #9931, .T. ) ;
#14937 = LINE ( 'NONE', #1698, #10614 ) ;
#14938 = ORIENTED_EDGE ( 'NONE', *, *, #3447, .F. ) ;
#14939 = CARTESIAN_POINT ( 'NONE',  ( -25.00000000000000000, 53.00000000000000711, -50.00000000000000000 ) ) ;
#14940 = CARTESIAN_POINT ( 'NONE',  ( -40.00000000000000711, 110.0000000000000000, 19.99999999999999645 ) ) ;
#14941 = CIRCLE ( 'NONE', #13358, 2.500000000000000444 ) ;
#14942 = DIRECTION ( 'NONE',  ( -0.000000000000000000, 1.000000000000000000, -0.000000000000000000 ) ) ;
#14943 = CARTESIAN_POINT ( 'NONE',  ( -25.00000000000000711, 110.0000000000000000, -6.000000000000001776 ) ) ;
#14944 = FACE_OUTER_BOUND ( 'NONE', #15102, .T. ) ;
#14945 = CARTESIAN_POINT ( 'NONE',  ( 2.066987300000001859, 63.14382582708704916, 47.70000000109246940 ) ) ;
#14946 = CARTESIAN_POINT ( 'NONE',  ( 1.767766952966369987, 65.76776695296638309, 45.69999999999999574 ) ) ;
#14947 = DIRECTION ( 'NONE',  ( -0.000000000000000000, -1.000000000000000000, -0.000000000000000000 ) ) ;
#14948 = EDGE_CURVE ( 'NONE', #9100, #17922, #16832, .T. ) ;
#14949 = ORIENTED_EDGE ( 'NONE', *, *, #10695, .F. ) ;
#14950 =( LENGTH_UNIT ( ) NAMED_UNIT ( * ) SI_UNIT ( .MILLI., .METRE. ) );
#14951 = CARTESIAN_POINT ( 'NONE',  ( -9.999999999999994671, -24.16482700510257686, 5.576177507916958653 ) ) ;
#14952 = CARTESIAN_POINT ( 'NONE',  ( -14.83517299489739649, -18.99999999999997868, 9.513677507916957765 ) ) ;
#14953 = CARTESIAN_POINT ( 'NONE',  ( -17.04047135212050890, -17.04416526290807710, 42.76757249208304046 ) ) ;
#14954 = CARTESIAN_POINT ( 'NONE',  ( -2.066987300000001859, 64.85617417291294373, 45.70000000109248361 ) ) ;
#14955 = CARTESIAN_POINT ( 'NONE',  ( -13.64274437364856141, -26.68048971390460622, 37.95117750791695244 ) ) ;
#14956 = CARTESIAN_POINT ( 'NONE',  ( -3.065533689247737392, -43.60761626555502346, 3.000000000000000000 ) ) ;
#14957 = CARTESIAN_POINT ( 'NONE',  ( -9.955834737091912245, -22.82508104294696238, 5.357427507916956877 ) ) ;
#14958 = CARTESIAN_POINT ( 'NONE',  ( 2.500000000000001776, 64.00000000000000000, 46.39999999999999858 ) ) ;
#14959 = CARTESIAN_POINT ( 'NONE',  ( 2.066987300000001859, 64.85617417291294373, 49.40000000109246514 ) ) ;
#14960 = DIRECTION ( 'NONE',  ( 0.000000000000000000, -1.000000000000000000, 0.000000000000000000 ) ) ;
#14961 = DIRECTION ( 'NONE',  ( 0.000000000000000000, -1.000000000000000000, 0.000000000000000000 ) ) ;
#14962 = CARTESIAN_POINT ( 'NONE',  ( -41.00000000000000711, 110.0000000000000000, -11.50000000000000355 ) ) ;
#14963 = CARTESIAN_POINT ( 'NONE',  ( -24.00000000000000000, 53.00000000000000711, 8.000000000000000000 ) ) ;
#14964 = EDGE_CURVE ( 'NONE', #3236, #17673, #13580, .T. ) ;
#14965 = DIRECTION ( 'NONE',  ( 1.000000000000000000, 0.000000000000000000, 0.000000000000000000 ) ) ;
#14967 = VERTEX_POINT ( 'NONE', #12313 ) ;
#14966 = EDGE_CURVE ( 'NONE', #14005, #6936, #7812, .T. ) ;
#14968 = ORIENTED_EDGE ( 'NONE', *, *, #1295, .T. ) ;
#14969 = CARTESIAN_POINT ( 'NONE',  ( -22.04416526290809486, -22.28918265808477628, 20.89257249208303691 ) ) ;
#14970 =( NAMED_UNIT ( * ) SI_UNIT ( $, .STERADIAN. ) SOLID_ANGLE_UNIT ( ) );
#14971 = CARTESIAN_POINT ( 'NONE',  ( -41.00000000000000711, 110.0000000000000000, -24.49999999999999645 ) ) ;
#14973 = ORIENTED_EDGE ( 'NONE', *, *, #16339, .T. ) ;
#14972 = EDGE_LOOP ( 'NONE', ( #13495, #4401, #6032, #14404, #7256 ) ) ;
#14974 = CARTESIAN_POINT ( 'NONE',  ( -12.92450931948788906, -26.31681416490114245, 11.48242750791695954 ) ) ;
#14975 = DIRECTION ( 'NONE',  ( 1.000000000000000000, 0.000000000000000000, 0.000000000000000000 ) ) ;
#14976 = CARTESIAN_POINT ( 'NONE',  ( -11.64274437364859693, -17.85540867095757989, 1.423822492083038904 ) ) ;
#14977 = CARTESIAN_POINT ( 'NONE',  ( 2.066987300000001859, 64.85617417291294373, 49.20000000109247651 ) ) ;
#14978 = CARTESIAN_POINT ( 'NONE',  ( 2.500000000000001776, 64.00000000000000000, 44.90000000218493881 ) ) ;
#14979 = EDGE_LOOP ( 'NONE', ( #11177, #11620, #3231, #1651 ) ) ;
#14980 = ORIENTED_EDGE ( 'NONE', *, *, #8755, .F. ) ;
#14981 = AXIS2_PLACEMENT_3D ( 'NONE', #10833, #12600, #2118 ) ;
#14982 = CARTESIAN_POINT ( 'NONE',  ( -2.081668171172168513E-14, 16.06586399182267755, 70.06586399182252478 ) ) ;
#14983 = EDGE_LOOP ( 'NONE', ( #11457, #16869, #14673, #15969 ) ) ;
#14984 = LINE ( 'NONE', #186, #11219 ) ;
#14985 = PLANE ( 'NONE',  #13291 ) ;
#14986 = CARTESIAN_POINT ( 'NONE',  ( -1.265664690411616068E-16, 66.06698730000000808, 47.95000000109246940 ) ) ;
#14987 = CARTESIAN_POINT ( 'NONE',  ( 4.101219330881941794, 26.84264068711924267, 59.64264068711931088 ) ) ;
#14988 = EDGE_CURVE ( 'NONE', #1673, #7148, #12409, .T. ) ;
#14989 = LINE ( 'NONE', #14600, #15517 ) ;
#14990 = ORIENTED_EDGE ( 'NONE', *, *, #6035, .T. ) ;
#14992 = ORIENTED_EDGE ( 'NONE', *, *, #18936, .T. ) ;
#14991 = EDGE_LOOP ( 'NONE', ( #16246, #16678 ) ) ;
#14993 = CARTESIAN_POINT ( 'NONE',  ( -9.020235676060220698, -27.64274437364852588, 11.26367750791695599 ) ) ;
#14994 = CIRCLE ( 'NONE', #12782, 0.1499999999999999667 ) ;
#14995 = DIRECTION ( 'NONE',  ( 0.000000000000000000, -1.000000000000000000, 0.000000000000000000 ) ) ;
#14996 = EDGE_LOOP ( 'NONE', ( #16863, #12891 ) ) ;
#14997 = VERTEX_POINT ( 'NONE', #4679 ) ;
#14998 = CARTESIAN_POINT ( 'NONE',  ( -15.16482700510262482, -20.99999999999997513, 11.48632249208304223 ) ) ;
#14999 = EDGE_CURVE ( 'NONE', #8051, #16200, #163, .T. ) ;
#15000 =( BOUNDED_CURVE ( )  B_SPLINE_CURVE ( 2, ( #8789, #4192, #6056, #17615, #7320, #7622, #4391, #10446, #5858 ),
 .UNSPECIFIED., .F., .F. ) 
 B_SPLINE_CURVE_WITH_KNOTS ( ( 3, 2, 2, 2, 3 ),
 ( 0.4285714285714284921, 0.4464285714285714524, 0.4642857142857143016, 0.4821428571428572063, 0.5000000000000001110 ),
 .UNSPECIFIED. ) 
 CURVE ( )  GEOMETRIC_REPRESENTATION_ITEM ( )  RATIONAL_B_SPLINE_CURVE ( ( 1.000000000000000222, 0.9238795325112865164, 1.000000000000000000, 0.9238795325112867385, 1.000000000000000000, 0.9238795325112867385, 1.000000000000000000, 0.9238795325112862944, 1.000000000000000444 ) ) 
 REPRESENTATION_ITEM ( '' )  );
#15001 = LINE ( 'NONE', #2842, #19084 ) ;
#15002 = CARTESIAN_POINT ( 'NONE',  ( -32.50000000000000000, 53.00000000000000711, -35.00000000000000000 ) ) ;
#15003 = VERTEX_POINT ( 'NONE', #18407 ) ;
#15004 = CARTESIAN_POINT ( 'NONE',  ( -14.83517299489738761, -20.99999999999997513, 20.01367750791696309 ) ) ;
#15005 = VECTOR ( 'NONE', #18328, 1000.000000000000000 ) ;
#15006 = CARTESIAN_POINT ( 'NONE',  ( -41.00000000000000711, 53.00000000000000711, 20.00000000000000000 ) ) ;
#15007 = ORIENTED_EDGE ( 'NONE', *, *, #15732, .F. ) ;
#15008 = PLANE ( 'NONE',  #8756 ) ;
#15009 = ORIENTED_EDGE ( 'NONE', *, *, #3418, .T. ) ;
#15010 = CARTESIAN_POINT ( 'NONE',  ( -41.00000000000000711, 53.00000000000000711, -12.50000000000000000 ) ) ;
#15011 = CARTESIAN_POINT ( 'NONE',  ( 2.500000000000001776, 64.00000000000000000, 45.70000000218494307 ) ) ;
#15012 = AXIS2_PLACEMENT_3D ( 'NONE', #16107, #5338, #4049 ) ;
#15013 = PLANE ( 'NONE',  #1931 ) ;
#15014 = VECTOR ( 'NONE', #592, 1000.000000000000000 ) ;
#15015 = SHAPE_DEFINITION_REPRESENTATION ( #3936, #13906 ) ;
#15016 = LINE ( 'NONE', #7366, #3509 ) ;
#15017 = CARTESIAN_POINT ( 'NONE',  ( -19.24771351637089367, -21.35725562635142438, 34.88867750791696665 ) ) ;
#15018 = ADVANCED_FACE ( 'NONE', ( #3496 ), #6537, .F. ) ;
#15019 =( NAMED_UNIT ( * ) SI_UNIT ( $, .STERADIAN. ) SOLID_ANGLE_UNIT ( ) );
#15020 = EDGE_CURVE ( 'NONE', #7828, #17265, #18308, .T. ) ;
#15021 = CARTESIAN_POINT ( 'NONE',  ( -16.50457296725820555, -28.95583473709189448, 17.60742750791695599 ) ) ;
#15022 = EDGE_CURVE ( 'NONE', #4615, #111, #10930, .T. ) ;
#15023 = VECTOR ( 'NONE', #1175, 1000.000000000000114 ) ;
#15024 = LINE ( 'NONE', #14927, #9579 ) ;
#15025 = ORIENTED_EDGE ( 'NONE', *, *, #15732, .T. ) ;
#15026 = CARTESIAN_POINT ( 'NONE',  ( -19.99999999999999645, -24.16482700510261949, 20.67382249208304401 ) ) ;
#15027 = TOROIDAL_SURFACE ( 'NONE', #2795, 2.700000000000000622, 0.2000000000000000111 ) ;
#15028 = CARTESIAN_POINT ( 'NONE',  ( -2.066987300000001859, 64.85617417291294373, 45.50000000109247367 ) ) ;
#15029 = CARTESIAN_POINT ( 'NONE',  ( -17.31681416490117087, -21.92450931948788551, 10.83007249208304223 ) ) ;
#15030 = VERTEX_POINT ( 'NONE', #9468 ) ;
#15031 = VECTOR ( 'NONE', #13914, 1000.000000000000000 ) ;
#15032 = DIRECTION ( 'NONE',  ( 0.000000000000000000, -1.000000000000000000, 0.000000000000000000 ) ) ;
#15033 = EDGE_LOOP ( 'NONE', ( #9333, #17248, #16250, #18815 ) ) ;
#15034 = DIRECTION ( 'NONE',  ( 0.000000000000000000, 0.000000000000000000, -1.000000000000000000 ) ) ;
#15035 = CARTESIAN_POINT ( 'NONE',  ( 5.199999999999996625, 3.061616997868383634E-16, -2.500000000000000444 ) ) ;
#15036 = CARTESIAN_POINT ( 'NONE',  ( 1.300000000000000044, 0.000000000000000000, 0.000000000000000000 ) ) ;
#15037 = DIRECTION ( 'NONE',  ( -0.000000000000000000, -0.000000000000000000, -1.000000000000000000 ) ) ;
#15038 = VECTOR ( 'NONE', #18892, 1000.000000000000000 ) ;
#15039 = CARTESIAN_POINT ( 'NONE',  ( -2.066987300000001415, 64.00000000000000000, 47.35000000109246798 ) ) ;
#15040 = VECTOR ( 'NONE', #8722, 1000.000000000000000 ) ;
#15041 = ADVANCED_FACE ( 'NONE', ( #10636 ), #18211, .F. ) ;
#15042 = CARTESIAN_POINT ( 'NONE',  ( -2.500000000000001776, 65.03553390593273775, 45.95000000000000995 ) ) ;
#15043 = DIRECTION ( 'NONE',  ( -0.000000000000000000, -0.000000000000000000, -1.000000000000000000 ) ) ;
#15044 = VECTOR ( 'NONE', #19345, 1000.000000000000000 ) ;
#15045 = ORIENTED_EDGE ( 'NONE', *, *, #12010, .T. ) ;
#15046 = EDGE_CURVE ( 'NONE', #587, #18462, #551, .T. ) ;
#15047 = DIRECTION ( 'NONE',  ( 1.000000000000000000, 0.000000000000000000, 0.000000000000000000 ) ) ;
#15048 = VECTOR ( 'NONE', #5824, 1000.000000000000000 ) ;
#15049 = CARTESIAN_POINT ( 'NONE',  ( -13.82508104294698192, -29.04416526290806644, 22.41992750791695244 ) ) ;
#15050 = CARTESIAN_POINT ( 'NONE',  ( -17.64274437364855430, -28.24771351637087236, 12.57617750791695777 ) ) ;
#15051 = CARTESIAN_POINT ( 'NONE',  ( -2.019187605927083240, 65.02780627284310810, 45.00000000000004263 ) ) ;
#15052 = CARTESIAN_POINT ( 'NONE',  ( -15.16482700510263371, -18.99999999999997868, 0.9863224920830410136 ) ) ;
#15053 = VECTOR ( 'NONE', #3449, 1000.000000000000000 ) ;
#15054 = DIRECTION ( 'NONE',  ( 0.000000000000000000, 0.000000000000000000, -1.000000000000000000 ) ) ;
#15055 = CARTESIAN_POINT ( 'NONE',  ( -20.04416526290808065, -25.17491895705300209, 2.732427507916957765 ) ) ;
#15056 = DIRECTION ( 'NONE',  ( 0.000000000000000000, 0.000000000000000000, 1.000000000000000000 ) ) ;
#15057 = CARTESIAN_POINT ( 'NONE',  ( -19.24771351637089367, -21.35725562635142438, 24.38867750791695954 ) ) ;
#15058 = DIRECTION ( 'NONE',  ( 1.000000000000000000, 0.000000000000000000, 0.000000000000000000 ) ) ;
#15059 = VECTOR ( 'NONE', #6195, 1000.000000000000000 ) ;
#15060 = EDGE_CURVE ( 'NONE', #10380, #12337, #15259, .T. ) ;
#15061 = CARTESIAN_POINT ( 'NONE',  ( -0.8561741729129461742, 66.06698729999999387, 49.60000000109246798 ) ) ;
#15062 = FACE_OUTER_BOUND ( 'NONE', #5558, .T. ) ;
#15063 = CARTESIAN_POINT ( 'NONE',  ( 44.99999999999998579, 6.000000000000000000, -54.99999999999998579 ) ) ;
#15064 = VECTOR ( 'NONE', #11668, 1000.000000000000000 ) ;
#15065 = DIRECTION ( 'NONE',  ( 0.000000000000000000, 0.000000000000000000, 1.000000000000000000 ) ) ;
#15066 = CARTESIAN_POINT ( 'NONE',  ( -2.066987300000001859, 64.85617417291294373, 49.70000000109248361 ) ) ;
#15067 = CARTESIAN_POINT ( 'NONE',  ( -25.00000000000000711, 53.00000000000000711, -30.99999999999999645 ) ) ;
#15068 = VECTOR ( 'NONE', #2001, 1000.000000000000000 ) ;
#15069 = DIRECTION ( 'NONE',  ( -1.000000000000000000, 0.000000000000000000, 0.000000000000000000 ) ) ;
#15070 = ORIENTED_EDGE ( 'NONE', *, *, #16910, .F. ) ;
#15071 = EDGE_CURVE ( 'NONE', #1832, #17252, #3096, .T. ) ;
#15072 = VERTEX_POINT ( 'NONE', #18694 ) ;
#15073 = CARTESIAN_POINT ( 'NONE',  ( -9.020235676060250896, -20.35725562635137820, 17.61132249208303335 ) ) ;
#15074 = VECTOR ( 'NONE', #5366, 1000.000000000000000 ) ;
#15075 = LINE ( 'NONE', #2811, #4737 ) ;
#15077 = VERTEX_POINT ( 'NONE', #11400 ) ;
#15076 = EDGE_LOOP ( 'NONE', ( #4120, #3599, #1899, #11855 ) ) ;
#15078 = CARTESIAN_POINT ( 'NONE',  ( -17.51566270880201159, -22.35725562635141728, 13.88867750791695954 ) ) ;
#15079 = DIRECTION ( 'NONE',  ( 0.000000000000000000, 0.000000000000000000, -1.000000000000000000 ) ) ;
#15080 = CARTESIAN_POINT ( 'NONE',  ( -7.999999999999996447, -23.83517299489733432, 2.298822492083038682 ) ) ;
#15081 = VECTOR ( 'NONE', #6345, 1000.000000000000000 ) ;
#15082 = CARTESIAN_POINT ( 'NONE',  ( -1.530808498934192803E-16, 66.50000000000000000, 48.19999999999999574 ) ) ;
#15083 = CARTESIAN_POINT ( 'NONE',  ( -0.8561741729129465073, 61.93301270000000613, 47.30000000109247082 ) ) ;
#15084 = VERTEX_POINT ( 'NONE', #9753 ) ;
#15085 = ORIENTED_EDGE ( 'NONE', *, *, #2297, .T. ) ;
#15086 = STYLED_ITEM ( 'NONE', ( #9910 ), #10198 ) ;
#15087 = CARTESIAN_POINT ( 'NONE',  ( -31.74999999999995737, 0.000000000000000000, 1.500000000000000222 ) ) ;
#15088 = LINE ( 'NONE', #10459, #3837 ) ;
#15089 = ORIENTED_EDGE ( 'NONE', *, *, #1135, .F. ) ;
#15090 = CARTESIAN_POINT ( 'NONE',  ( -10.71682923056184400, -22.10758631096295801, 1.196196559314993540E-16 ) ) ;
#15091 = CARTESIAN_POINT ( 'NONE',  ( -41.00000000000000711, 110.0000000000000000, -11.50000000000000000 ) ) ;
#15092 = CARTESIAN_POINT ( 'NONE',  ( 2.066987300000001415, 64.00000000000000000, 48.55000000109247082 ) ) ;
#15093 = APPLICATION_CONTEXT ( 'automotive_design' ) ;
#15094 = LINE ( 'NONE', #10466, #12546 ) ;
#15095 = LINE ( 'NONE', #16961, #7703 ) ;
#15096 = ORIENTED_EDGE ( 'NONE', *, *, #861, .F. ) ;
#15098 = ORIENTED_EDGE ( 'NONE', *, *, #11028, .T. ) ;
#15097 = VERTEX_POINT ( 'NONE', #5445 ) ;
#15099 = CARTESIAN_POINT ( 'NONE',  ( -18.64274437364853654, -29.97976432393976509, 12.57617750791695599 ) ) ;
#15100 = AXIS2_PLACEMENT_3D ( 'NONE', #10829, #6142, #12203 ) ;
#15101 = DIRECTION ( 'NONE',  ( 0.000000000000000000, 0.000000000000000000, 1.000000000000000000 ) ) ;
#15102 = EDGE_LOOP ( 'NONE', ( #4443, #6778, #4351, #12255 ) ) ;
#15103 = ORIENTED_EDGE ( 'NONE', *, *, #9023, .T. ) ;
#15104 = CARTESIAN_POINT ( 'NONE',  ( -14.03132541760400009, -26.95583473709189448, 19.14257249208304401 ) ) ;
#15105 = CARTESIAN_POINT ( 'NONE',  ( -2.066987300000000971, 63.14382582708704916, 48.80000000109247082 ) ) ;
#15106 = DIRECTION ( 'NONE',  ( 0.000000000000000000, -0.7071067811865456854, -0.7071067811865493491 ) ) ;
#15107 = VERTEX_POINT ( 'NONE', #2490 ) ;
#15108 = CARTESIAN_POINT ( 'NONE',  ( -17.07549068051210739, -21.68318583509881847, 14.10742750791695954 ) ) ;
#15109 = LINE ( 'NONE', #9122, #15995 ) ;
#15110 = ORIENTED_EDGE ( 'NONE', *, *, #5891, .T. ) ;
#15111 = LINE ( 'NONE', #13328, #2499 ) ;
#15112 = ORIENTED_EDGE ( 'NONE', *, *, #2657, .T. ) ;
#15113 = CARTESIAN_POINT ( 'NONE',  ( -1.530808498934192803E-16, 66.50000000000000000, 46.59999999999999432 ) ) ;
#15114 = CARTESIAN_POINT ( 'NONE',  ( -41.00000000000000711, 110.0000000000000000, 27.50000000000000000 ) ) ;
#15115 = LINE ( 'NONE', #16282, #11295 ) ;
#15116 = DIRECTION ( 'NONE',  ( 0.000000000000000000, -0.5000000000000013323, -0.8660254037844380415 ) ) ;
#15117 = LINE ( 'NONE', #10396, #11011 ) ;
#15118 = EDGE_CURVE ( 'NONE', #8404, #1836, #8207, .T. ) ;
#15119 = EDGE_CURVE ( 'NONE', #13223, #18899, #6910, .T. ) ;
#15120 = CARTESIAN_POINT ( 'NONE',  ( -1.035533905932738641, 66.50000000000000000, 48.24999999999999289 ) ) ;
#15121 = DIRECTION ( 'NONE',  ( 0.000000000000000000, 0.000000000000000000, 1.000000000000000000 ) ) ;
#15123 = EDGE_CURVE ( 'NONE', #13902, #17838, #5258, .T. ) ;
#15122 = CARTESIAN_POINT ( 'NONE',  ( -18.53959229564986799, -20.21908421996107563, 19.35742750791695599 ) ) ;
#15124 = PLANE ( 'NONE',  #4918 ) ;
#15125 = ORIENTED_EDGE ( 'NONE', *, *, #3494, .F. ) ;
#15126 = CARTESIAN_POINT ( 'NONE',  ( -14.83517299489735741, -28.99999999999998224, 19.36132249208304046 ) ) ;
#15127 = EDGE_CURVE ( 'NONE', #19340, #2343, #8290, .T. ) ;
#15128 = LINE ( 'NONE', #2340, #3814 ) ;
#15129 = CARTESIAN_POINT ( 'NONE',  ( -14.83517299489736985, -26.99999999999998579, 24.61132249208304756 ) ) ;
#15130 = DIRECTION ( 'NONE',  ( 0.000000000000000000, -0.4999999999999992784, 0.8660254037844390407 ) ) ;
#15131 = ORIENTED_EDGE ( 'NONE', *, *, #13910, .F. ) ;
#15132 = CARTESIAN_POINT ( 'NONE',  ( 21.50000000000001421, 118.0000000000000142, 32.49999999999998579 ) ) ;
#15133 = ORIENTED_EDGE ( 'NONE', *, *, #189, .F. ) ;
#15134 = DIRECTION ( 'NONE',  ( 3.826732013112563602E-16, -1.000000000000000000, 0.000000000000000000 ) ) ;
#15135 = EDGE_CURVE ( 'NONE', #5010, #908, #2122, .T. ) ;
#15136 = CARTESIAN_POINT ( 'NONE',  ( -37.50000000000002132, -6.000000000000000000, 24.99999999999998224 ) ) ;
#15137 = DIRECTION ( 'NONE',  ( -0.000000000000000000, -0.000000000000000000, -1.000000000000000000 ) ) ;
#15138 = CARTESIAN_POINT ( 'NONE',  ( 2.066987300000001415, 64.00000000000000000, 46.15000000109247225 ) ) ;
#15139 = CARTESIAN_POINT ( 'NONE',  ( -40.00000000000000000, 53.00000000000000711, 30.00000000000000000 ) ) ;
#15140 = EDGE_CURVE ( 'NONE', #76, #11826, #8106, .T. ) ;
#15141 = CARTESIAN_POINT ( 'NONE',  ( 41.99999999999998579, 6.000000000000005329, -52.00000000000000000 ) ) ;
#15142 = DIRECTION ( 'NONE',  ( -1.000000000000000000, -0.000000000000000000, -0.000000000000000000 ) ) ;
#15143 = VERTEX_POINT ( 'NONE', #15553 ) ;
#15144 = DIRECTION ( 'NONE',  ( 0.000000000000000000, 0.000000000000000000, 1.000000000000000000 ) ) ;
#15145 = CARTESIAN_POINT ( 'NONE',  ( -19.95583473709191580, -22.49542703274176603, 24.16992750791694888 ) ) ;
#15146 = CARTESIAN_POINT ( 'NONE',  ( -1.767766952966369765, 62.23223304703363112, 47.80000000218494449 ) ) ;
#15147 = CARTESIAN_POINT ( 'NONE',  ( -13.49542703274174116, -28.95583473709188738, 24.39257249208303335 ) ) ;
#15148 = EDGE_CURVE ( 'NONE', #13491, #1736, #2215, .T. ) ;
#15149 = EDGE_CURVE ( 'NONE', #18134, #3857, #12882, .T. ) ;
#15150 = CARTESIAN_POINT ( 'NONE',  ( 0.8561741729129460632, 66.06698729999999387, 46.30000000109247082 ) ) ;
#15151 = CARTESIAN_POINT ( 'NONE',  ( -17.95583473709191580, -23.03132541760400898, 39.91992750791695954 ) ) ;
#15152 = EDGE_CURVE ( 'NONE', #11826, #1662, #1029, .T. ) ;
#15153 = FACE_OUTER_BOUND ( 'NONE', #7297, .T. ) ;
#15154 = CARTESIAN_POINT ( 'NONE',  ( -9.955834737091912245, -22.82508104294696238, 21.10742750791695599 ) ) ;
#15155 = DIRECTION ( 'NONE',  ( -7.709882115452476934E-17, -0.000000000000000000, -1.000000000000000000 ) ) ;
#15156 = FACE_BOUND ( 'NONE', #15267, .T. ) ;
#15157 = EDGE_CURVE ( 'NONE', #17823, #7137, #14076, .T. ) ;
#15158 = CARTESIAN_POINT ( 'NONE',  ( -2.066987300000001415, 63.14382582708705627, 46.60000000109246088 ) ) ;
#15159 = PLANE ( 'NONE',  #2766 ) ;
#15160 = PLANE ( 'NONE',  #15712 ) ;
#15161 = DIRECTION ( 'NONE',  ( 0.000000000000000000, 0.000000000000000000, -1.000000000000000000 ) ) ;
#15162 = LINE ( 'NONE', #1538, #4742 ) ;
#15163 = DIRECTION ( 'NONE',  ( 1.000000000000000000, -0.000000000000000000, -0.000000000000000000 ) ) ;
#15164 = B_SPLINE_CURVE_WITH_KNOTS ( 'NONE', 3,
 ( #11896, #14645, #8570, #4363 ),
 .UNSPECIFIED., .F., .F.,
 ( 4, 4 ),
 ( 0.000000000000000000, 1.000000000000000000 ),
 .UNSPECIFIED. ) ;
#15165 = AXIS2_PLACEMENT_3D ( 'NONE', #15139, #6029, #13462 ) ;
#15166 = PLANE ( 'NONE',  #12073 ) ;
#15167 = VERTEX_POINT ( 'NONE', #18882 ) ;
#15168 = ORIENTED_EDGE ( 'NONE', *, *, #14636, .T. ) ;
#15169 = CARTESIAN_POINT ( 'NONE',  ( -9.754982604823302594, -29.00369391078756465, 13.45507249208303868 ) ) ;
#15170 =( LENGTH_UNIT ( ) NAMED_UNIT ( * ) SI_UNIT ( .MILLI., .METRE. ) );
#15171 = CARTESIAN_POINT ( 'NONE',  ( -18.78091578003892792, -20.46040770435013556, 10.83007249208303868 ) ) ;
#15173 = ORIENTED_EDGE ( 'NONE', *, *, #11069, .T. ) ;
#15172 = ORIENTED_EDGE ( 'NONE', *, *, #9886, .F. ) ;
#15174 = EDGE_CURVE ( 'NONE', #12045, #375, #9837, .T. ) ;
#15175 = CARTESIAN_POINT ( 'NONE',  ( -15.63902057219076269, -20.95583473709189448, 14.54492750791695954 ) ) ;
#15176 = DIRECTION ( 'NONE',  ( 0.000000000000000000, 0.000000000000000000, 1.000000000000000000 ) ) ;
#15177 = CARTESIAN_POINT ( 'NONE',  ( -20.97976432393974022, -27.64274437364858628, 25.48632249208304401 ) ) ;
#15178 = CARTESIAN_POINT ( 'NONE',  ( -1.461580736456473906, 65.46158073645646880, 48.65000000109247225 ) ) ;
#15179 = CARTESIAN_POINT ( 'NONE',  ( -2.066987300000001415, 63.14382582708705627, 47.20000000109248361 ) ) ;
#15180 = EDGE_LOOP ( 'NONE', ( #3432, #18446, #3892, #2258 ) ) ;
#15181 = ORIENTED_EDGE ( 'NONE', *, *, #18393, .T. ) ;
#15182 = DIRECTION ( 'NONE',  ( 1.000000000000000000, 0.000000000000000000, 2.973811673103096679E-16 ) ) ;
#15183 = ORIENTED_EDGE ( 'NONE', *, *, #19206, .T. ) ;
#15184 = VECTOR ( 'NONE', #10431, 1000.000000000000000 ) ;
#15185 = VERTEX_POINT ( 'NONE', #17217 ) ;
#15186 = CARTESIAN_POINT ( 'NONE',  ( -4.999999999999980460, 0.000000000000000000, 69.99999999999998579 ) ) ;
#15187 = LINE ( 'NONE', #16428, #13430 ) ;
#15188 = PLANE ( 'NONE',  #13485 ) ;
#15189 = PLANE ( 'NONE',  #11920 ) ;
#15190 = CARTESIAN_POINT ( 'NONE',  ( -41.00000000000000711, 53.00000000000000711, 1.500000000000001332 ) ) ;
#15191 = VERTEX_POINT ( 'NONE', #8382 ) ;
#15193 = ORIENTED_EDGE ( 'NONE', *, *, #5989, .F. ) ;
#15192 = EDGE_LOOP ( 'NONE', ( #17707, #1148, #14949, #2932 ) ) ;
#15194 = CARTESIAN_POINT ( 'NONE',  ( -15.16482700510258574, -30.99999999999998224, 17.38867750791695599 ) ) ;
#15195 = PRODUCT_DEFINITION_FORMATION_WITH_SPECIFIED_SOURCE ( 'ANY', '', #5998, .NOT_KNOWN. ) ;
#15196 =( LENGTH_UNIT ( ) NAMED_UNIT ( * ) SI_UNIT ( .MILLI., .METRE. ) );
#15197 = ORIENTED_EDGE ( 'NONE', *, *, #10385, .T. ) ;
#15198 = VECTOR ( 'NONE', #19230, 1000.000000000000000 ) ;
#15199 = ORIENTED_EDGE ( 'NONE', *, *, #17193, .F. ) ;
#15200 = EDGE_CURVE ( 'NONE', #856, #13243, #3784, .T. ) ;
#15201 = CARTESIAN_POINT ( 'NONE',  ( -12.48433729119799196, -22.35725562635139596, 12.36132249208304401 ) ) ;
#15202 = CARTESIAN_POINT ( 'NONE',  ( -18.35725562635144925, -17.85540867095761186, 3.826177507916956433 ) ) ;
#15203 = CARTESIAN_POINT ( 'NONE',  ( 1.461580736456473906, 62.53841926354353120, 47.45000000109246940 ) ) ;
#15204 = CARTESIAN_POINT ( 'NONE',  ( -45.00000000000000000, 3.000000000000000000, 53.39999999999999147 ) ) ;
#15205 = ORIENTED_EDGE ( 'NONE', *, *, #10219, .T. ) ;
#15206 = CARTESIAN_POINT ( 'NONE',  ( -15.16482700510260706, -26.99999999999998579, 22.63867750791696309 ) ) ;
#15207 = CARTESIAN_POINT ( 'NONE',  ( -1.040834085586084257E-14, 32.57106781186548972, 45.42893218813454581 ) ) ;
#15208 = ORIENTED_EDGE ( 'NONE', *, *, #1859, .T. ) ;
#15209 = LINE ( 'NONE', #495, #18495 ) ;
#15210 = EDGE_LOOP ( 'NONE', ( #16666, #11237, #4836, #17828 ) ) ;
#15211 = SURFACE_STYLE_USAGE ( .BOTH. , #9220 ) ;
#15212 = FACE_BOUND ( 'NONE', #14200, .T. ) ;
#15213 = FACE_OUTER_BOUND ( 'NONE', #5981, .T. ) ;
#15214 = VECTOR ( 'NONE', #6858, 1000.000000000000000 ) ;
#15215 = DIRECTION ( 'NONE',  ( -7.709882115452476934E-17, -0.000000000000000000, -1.000000000000000000 ) ) ;
#15216 = VECTOR ( 'NONE', #15079, 1000.000000000000000 ) ;
#15217 = CARTESIAN_POINT ( 'NONE',  ( 14.99999999999998579, 52.00000000000000711, 23.99999999999997158 ) ) ;
#15218 = LINE ( 'NONE', #6299, #14413 ) ;
#15219 = CARTESIAN_POINT ( 'NONE',  ( -19.95583473709191580, -22.49542703274176603, 34.66992750791694533 ) ) ;
#15220 = DIRECTION ( 'NONE',  ( -1.000000000000000000, 0.000000000000000000, -0.000000000000000000 ) ) ;
#15221 = ORIENTED_EDGE ( 'NONE', *, *, #14193, .F. ) ;
#15222 = CARTESIAN_POINT ( 'NONE',  ( -12.35725562635143682, -19.75228648362908501, 9.951177507916959541 ) ) ;
#15223 = DIRECTION ( 'NONE',  ( -0.000000000000000000, -0.000000000000000000, -1.000000000000000000 ) ) ;
#15224 = ORIENTED_EDGE ( 'NONE', *, *, #12750, .T. ) ;
#15225 = CARTESIAN_POINT ( 'NONE',  ( -19.24771351637086880, -26.64274437364857206, 20.23632249208304046 ) ) ;
#15226 = CIRCLE ( 'NONE', #815, 4.250000000000000000 ) ;
#15227 = CARTESIAN_POINT ( 'NONE',  ( 5.800448837981379668, 29.71286850494547593, 56.77177811653250217 ) ) ;
#15228 = CARTESIAN_POINT ( 'NONE',  ( -11.95583473709190514, -24.63902057219072361, 13.01757249208304401 ) ) ;
#15229 = FACE_OUTER_BOUND ( 'NONE', #14394, .T. ) ;
#15230 = EDGE_LOOP ( 'NONE', ( #2710, #2885, #4294, #11879 ) ) ;
#15231 = PLANE ( 'NONE',  #5313 ) ;
#15232 = ORIENTED_EDGE ( 'NONE', *, *, #14270, .T. ) ;
#15233 = CARTESIAN_POINT ( 'NONE',  ( -9.698045712355376814E-15, 25.64142135623727370, 60.84386001800126564 ) ) ;
#15234 = CARTESIAN_POINT ( 'NONE',  ( -2.750000000000020872, 118.0000000000000142, -42.68883962248118991 ) ) ;
#15235 = CARTESIAN_POINT ( 'NONE',  ( -41.00000000000000711, 53.00000000000000711, -12.50000000000000000 ) ) ;
#15236 = CARTESIAN_POINT ( 'NONE',  ( -0.8561741729129461742, 66.06698730000000808, 44.80000000109246372 ) ) ;
#15237 = VECTOR ( 'NONE', #18692, 1000.000000000000000 ) ;
#15238 = LINE ( 'NONE', #1806, #457 ) ;
#15239 = DIRECTION ( 'NONE',  ( 2.775557561562890858E-16, 0.7071067811865454633, 0.7071067811865496822 ) ) ;
#15240 = VERTEX_POINT ( 'NONE', #15834 ) ;
#15241 = DIRECTION ( 'NONE',  ( 1.000000000000000000, 0.000000000000000000, 0.000000000000000000 ) ) ;
#15242 = CARTESIAN_POINT ( 'NONE',  ( -17.35725562635144215, -19.58745947852648683, 14.32617750791695777 ) ) ;
#15243 = CARTESIAN_POINT ( 'NONE',  ( -1.530808498934192803E-16, 66.50000000000000000, 45.10000000218494165 ) ) ;
#15244 = EDGE_CURVE ( 'NONE', #13749, #5786, #9560, .T. ) ;
#15245 = CARTESIAN_POINT ( 'NONE',  ( -18.53959229564982536, -27.78091578003890660, 20.01757249208304046 ) ) ;
#15246 = COLOUR_RGB ( '', 0.72549020, 0.75294118, 0.79215686) ;
#15247 = AXIS2_PLACEMENT_3D ( 'NONE', #2587, #11398, #8476 ) ;
#15248 = CARTESIAN_POINT ( 'NONE',  ( 2.500000000000000000, 2.357898499370431722, -2.818925648462311528E-15 ) ) ;
#15249 = CARTESIAN_POINT ( 'NONE',  ( -9.955834737091912245, -22.82508104294696594, 10.60742750791695777 ) ) ;
#15250 = CARTESIAN_POINT ( 'NONE',  ( -5.800000000000006928, 29.47747564417435484, 56.65425233947093631 ) ) ;
#15251 = CARTESIAN_POINT ( 'NONE',  ( -19.24771351637089367, -21.35725562635142438, 19.13867750791695954 ) ) ;
#15252 = CYLINDRICAL_SURFACE ( 'NONE', #5911, 2.500000000000001776 ) ;
#15253 = DIRECTION ( 'NONE',  ( 0.000000000000000000, 0.000000000000000000, 1.000000000000000000 ) ) ;
#15254 = CARTESIAN_POINT ( 'NONE',  ( -1.461580736456473906, 65.46158073645646880, 48.85000000109246798 ) ) ;
#15255 = PLANE ( 'NONE',  #10905 ) ;
#15256 = CARTESIAN_POINT ( 'NONE',  ( -12.50000000000000000, -35.50000000000000000, 5.000000000000003553 ) ) ;
#15257 = LINE ( 'NONE', #10928, #18697 ) ;
#15258 = CARTESIAN_POINT ( 'NONE',  ( -1.461580736456473462, 62.53841926354353120, 46.65000000109247225 ) ) ;
#15259 = LINE ( 'NONE', #10837, #7692 ) ;
#15260 = EDGE_CURVE ( 'NONE', #18667, #13252, #17309, .T. ) ;
#15261 = EDGE_CURVE ( 'NONE', #10270, #15191, #15226, .T. ) ;
#15262 = ORIENTED_EDGE ( 'NONE', *, *, #16694, .T. ) ;
#15263 = ORIENTED_EDGE ( 'NONE', *, *, #4104, .T. ) ;
#15264 = EDGE_CURVE ( 'NONE', #9938, #16495, #2399, .T. ) ;
#15265 = CARTESIAN_POINT ( 'NONE',  ( -9.996306089212408708, -18.75498260482328661, 38.39257249208304756 ) ) ;
#15266 = CARTESIAN_POINT ( 'NONE',  ( -15.16482700510263371, -18.99999999999997868, 16.73632249208304401 ) ) ;
#15267 = EDGE_LOOP ( 'NONE', ( #3246, #16647 ) ) ;
#15268 = CARTESIAN_POINT ( 'NONE',  ( -13.35725562635142794, -21.48433729119796709, 9.951177507916961318 ) ) ;
#15269 = CARTESIAN_POINT ( 'NONE',  ( -41.00000000000000711, 53.00000000000000711, -19.00000000000000000 ) ) ;
#15270 = CARTESIAN_POINT ( 'NONE',  ( -21.14459132904239169, -20.64274437364858628, 21.11132249208304046 ) ) ;
#15271 = DIRECTION ( 'NONE',  ( -0.000000000000000000, 1.000000000000000000, -0.000000000000000000 ) ) ;
#15272 = CARTESIAN_POINT ( 'NONE',  ( -0.8561741729129461742, 66.06698729999999387, 46.20000000109247651 ) ) ;
#15273 = EDGE_LOOP ( 'NONE', ( #5, #8233, #19385, #1147, #953 ) ) ;
#15274 = VERTEX_POINT ( 'NONE', #6815 ) ;
#15275 = PLANE ( 'NONE',  #3456 ) ;
#15276 = CARTESIAN_POINT ( 'NONE',  ( -2.500000000000001776, 64.00000000000000000, 49.99999999999999289 ) ) ;
#15277 = ORIENTED_EDGE ( 'NONE', *, *, #14337, .F. ) ;
#15278 = DIRECTION ( 'NONE',  ( -1.000000000000000000, -0.000000000000000000, -0.000000000000000000 ) ) ;
#15279 = DIRECTION ( 'NONE',  ( 0.000000000000000000, 0.000000000000000000, -1.000000000000000000 ) ) ;
#15280 = DIRECTION ( 'NONE',  ( -0.000000000000000000, -0.000000000000000000, -1.000000000000000000 ) ) ;
#15281 = CARTESIAN_POINT ( 'NONE',  ( 5.000000000000111910, 8.673617379884229532E-15, 69.99999999999998579 ) ) ;
#15282 = EDGE_CURVE ( 'NONE', #12144, #14297, #12781, .T. ) ;
#15283 = CARTESIAN_POINT ( 'NONE',  ( 2.500000000000002220, 62.96446609406726225, 45.65000000218494591 ) ) ;
#15284 = ORIENTED_EDGE ( 'NONE', *, *, #18144, .T. ) ;
#15286 = VERTEX_POINT ( 'NONE', #5927 ) ;
#15285 = ORIENTED_EDGE ( 'NONE', *, *, #8335, .T. ) ;
#15287 = CARTESIAN_POINT ( 'NONE',  ( -22.04416526290807710, -25.71081734191525925, 13.23242750791695777 ) ) ;
#15288 = SHAPE_REPRESENTATION ( 'Lever Press Handle Knob', ( #1791 ), #12745 ) ;
#15289 = CARTESIAN_POINT ( 'NONE',  ( 20.00000000000000355, 0.000000000000000000, 1.500000000000000000 ) ) ;
#15290 = VERTEX_POINT ( 'NONE', #10028 ) ;
#15291 = ORIENTED_EDGE ( 'NONE', *, *, #7786, .T. ) ;
#15292 = CARTESIAN_POINT ( 'NONE',  ( -16.35725562635141372, -26.68048971390461332, 14.54882249208304401 ) ) ;
#15293 = CARTESIAN_POINT ( 'NONE',  ( -18.35725562635144925, -17.85540867095761186, 14.32617750791695599 ) ) ;
#15294 = AXIS2_PLACEMENT_3D ( 'NONE', #10046, #16042, #846 ) ;
#15295 = CARTESIAN_POINT ( 'NONE',  ( 3.796994071234847710E-16, 61.93301269999999903, 48.95000000109246940 ) ) ;
#15296 = DIRECTION ( 'NONE',  ( -2.775557561562890858E-16, 0.7071067811865456854, 0.7071067811865493491 ) ) ;
#15297 = EDGE_LOOP ( 'NONE', ( #12742, #4202, #4132, #16303 ) ) ;
#15298 = CARTESIAN_POINT ( 'NONE',  ( -12.31951028609537602, -22.64274437364854364, 15.63867750791696309 ) ) ;
#15299 = ORIENTED_EDGE ( 'NONE', *, *, #1878, .F. ) ;
#15300 = CARTESIAN_POINT ( 'NONE',  ( -24.00000000000000000, 0.000000000000000000, -50.00000000000000000 ) ) ;
#15301 = ORIENTED_EDGE ( 'NONE', *, *, #17, .F. ) ;
#15302 = DIRECTION ( 'NONE',  ( -1.000000000000000000, 0.000000000000000000, -7.304098846218135653E-17 ) ) ;
#15303 = DIRECTION ( 'NONE',  ( 0.000000000000000000, -1.000000000000000000, -0.000000000000000000 ) ) ;
#15304 = FACE_OUTER_BOUND ( 'NONE', #4020, .T. ) ;
#15305 = DIRECTION ( 'NONE',  ( -1.000000000000000000, 0.000000000000000000, -0.000000000000000000 ) ) ;
#15306 = EDGE_CURVE ( 'NONE', #14701, #1350, #14549, .T. ) ;
#15307 = LINE ( 'NONE', #13731, #530 ) ;
#15308 = CARTESIAN_POINT ( 'NONE',  ( 11.00000000000000355, 0.000000000000000000, 0.000000000000000000 ) ) ;
#15309 = VECTOR ( 'NONE', #2990, 1000.000000000000000 ) ;
#15310 = CARTESIAN_POINT ( 'NONE',  ( 0.000000000000000000, 64.00000000000000000, 49.99999999999999289 ) ) ;
#15311 = FACE_OUTER_BOUND ( 'NONE', #10617, .T. ) ;
#15312 = VERTEX_POINT ( 'NONE', #4170 ) ;
#15313 = CARTESIAN_POINT ( 'NONE',  ( -10.58745947852649927, -21.64274437364853654, 20.88867750791695954 ) ) ;
#15314 = CARTESIAN_POINT ( 'NONE',  ( -2.315774708385978098, 27.80336399182263563, 58.32836399182264131 ) ) ;
#15315 = EDGE_LOOP ( 'NONE', ( #11442, #11498, #5465, #17510 ) ) ;
#15316 = CARTESIAN_POINT ( 'NONE',  ( -15.16482700510263371, -18.99999999999997868, 21.98632249208304401 ) ) ;
#15317 = EDGE_CURVE ( 'NONE', #6543, #17053, #8665, .T. ) ;
#15318 = VECTOR ( 'NONE', #18002, 1000.000000000000000 ) ;
#15319 = CARTESIAN_POINT ( 'NONE',  ( -15.63902057219073605, -27.04416526290807710, 14.33007249208304223 ) ) ;
#15320 = VECTOR ( 'NONE', #18449, 1000.000000000000000 ) ;
#15321 = ORIENTED_EDGE ( 'NONE', *, *, #11988, .T. ) ;
#15322 = CARTESIAN_POINT ( 'NONE',  ( -2.492551403682614186, 27.92836399182264273, 58.20336399182264131 ) ) ;
#15323 = ORIENTED_EDGE ( 'NONE', *, *, #12010, .F. ) ;
#15324 = FACE_OUTER_BOUND ( 'NONE', #174, .T. ) ;
#15325 = CARTESIAN_POINT ( 'NONE',  ( 0.000000000000000000, 0.000000000000000000, 9.500000000000001776 ) ) ;
#15326 = CARTESIAN_POINT ( 'NONE',  ( -1.485306817036799787, -32.00000000000000711, 3.500000000000006661 ) ) ;
#15327 = EDGE_CURVE ( 'NONE', #106, #15466, #19164, .T. ) ;
#15328 = LINE ( 'NONE', #18475, #15661 ) ;
#15329 = AXIS2_PLACEMENT_3D ( 'NONE', #16304, #7183, #6117 ) ;
#15330 = LINE ( 'NONE', #2000, #2023 ) ;
#15331 = CARTESIAN_POINT ( 'NONE',  ( -12.70357423236093197, -43.78611686177728046, 3.000000000000000000 ) ) ;
#15332 = CARTESIAN_POINT ( 'NONE',  ( -7.999999999999986677, 68.00000000000000000, 69.99999999999998579 ) ) ;
#15333 = VECTOR ( 'NONE', #15032, 1000.000000000000000 ) ;
#15334 = VECTOR ( 'NONE', #8902, 1000.000000000000000 ) ;
#15335 = ORIENTED_EDGE ( 'NONE', *, *, #9931, .F. ) ;
#15336 = DIRECTION ( 'NONE',  ( 1.000000000000000000, 0.000000000000000000, 0.000000000000000000 ) ) ;
#15337 = CARTESIAN_POINT ( 'NONE',  ( -12.64274437364855252, -28.41254052147347053, 16.95117750791695954 ) ) ;
#15338 = AXIS2_PLACEMENT_3D ( 'NONE', #864, #12725, #6843 ) ;
#15339 = CARTESIAN_POINT ( 'NONE',  ( -1.767766952966369765, 62.23223304703363112, 46.20000000218494307 ) ) ;
#15340 = CARTESIAN_POINT ( 'NONE',  ( -18.53959229564982536, -27.78091578003890660, 25.26757249208304401 ) ) ;
#15341 = VECTOR ( 'NONE', #5267, 1000.000000000000000 ) ;
#15342 = LINE ( 'NONE', #16918, #393 ) ;
#15343 = CARTESIAN_POINT ( 'NONE',  ( -20.04416526290808065, -25.17491895705300209, 13.23242750791695777 ) ) ;
#15344 = LINE ( 'NONE', #15445, #14863 ) ;
#15345 = CARTESIAN_POINT ( 'NONE',  ( -17.64274437364855430, -28.24771351637087236, 12.57617750791695777 ) ) ;
#15346 = AXIS2_PLACEMENT_3D ( 'NONE', #15967, #6947, #9787 ) ;
#15347 = CARTESIAN_POINT ( 'NONE',  ( 4.592425496802577917E-16, 61.50000000000000000, 46.99999999999999289 ) ) ;
#15348 = CARTESIAN_POINT ( 'NONE',  ( 2.500000000000001776, 64.00000000000000000, 45.59999999999999432 ) ) ;
#15349 = CARTESIAN_POINT ( 'NONE',  ( -0.8561741729129461742, 66.06698729999999387, 47.20000000109247651 ) ) ;
#15350 = CARTESIAN_POINT ( 'NONE',  ( -41.99999999999997868, 139.6861997365471950, 51.99999999999997868 ) ) ;
#15351 = CARTESIAN_POINT ( 'NONE',  ( -15.00000000000000000, 50.00000000000000000, 30.00000000000000000 ) ) ;
#15352 = AXIS2_PLACEMENT_3D ( 'NONE', #5620, #15563, #17672 ) ;
#15353 = DIRECTION ( 'NONE',  ( -0.000000000000000000, -0.000000000000000000, -1.000000000000000000 ) ) ;
#15354 = CARTESIAN_POINT ( 'NONE',  ( 2.066987300000001415, 64.00000000000000000, 49.35000000109246798 ) ) ;
#15355 = ADVANCED_FACE ( 'NONE', ( #10417 ), #1121, .F. ) ;
#15356 = EDGE_CURVE ( 'NONE', #9696, #11674, #10226, .T. ) ;
#15357 = DIRECTION ( 'NONE',  ( 0.000000000000000000, 0.8660254037844380415, -0.5000000000000009992 ) ) ;
#15358 = VECTOR ( 'NONE', #19328, 1000.000000000000000 ) ;
#15359 = EDGE_LOOP ( 'NONE', ( #4243, #480, #17453, #767 ) ) ;
#15360 = ORIENTED_EDGE ( 'NONE', *, *, #17296, .F. ) ;
#15361 = CARTESIAN_POINT ( 'NONE',  ( -7.999999999999996447, -23.83517299489733432, 39.04882249208302625 ) ) ;
#15362 = EDGE_CURVE ( 'NONE', #16765, #15802, #15164, .T. ) ;
#15363 = AXIS2_PLACEMENT_3D ( 'NONE', #5485, #15880, #7142 ) ;
#15364 =( NAMED_UNIT ( * ) SI_UNIT ( $, .STERADIAN. ) SOLID_ANGLE_UNIT ( ) );
#15365 = CARTESIAN_POINT ( 'NONE',  ( -10.75228648362912232, -21.35725562635138530, 12.36132249208304046 ) ) ;
#15366 = ORIENTED_EDGE ( 'NONE', *, *, #10910, .T. ) ;
#15367 = CARTESIAN_POINT ( 'NONE',  ( -12.04416526290807887, -24.96867458239596260, 32.04492750791695954 ) ) ;
#15368 = CARTESIAN_POINT ( 'NONE',  ( -37.50000000000002132, -6.000000000000000000, -25.00000000000002132 ) ) ;
#15369 = CARTESIAN_POINT ( 'NONE',  ( -20.00369391078757886, -29.24501739517668142, 14.76757249208304046 ) ) ;
#15370 = VECTOR ( 'NONE', #16357, 1000.000000000000000 ) ;
#15371 = CARTESIAN_POINT ( 'NONE',  ( 2.066987300000001415, 64.00000000000000000, 45.95000000109246940 ) ) ;
#15372 = CARTESIAN_POINT ( 'NONE',  ( -1.265664690411616068E-16, 66.06698730000000808, 46.15000000109247225 ) ) ;
#15373 = ORIENTED_EDGE ( 'NONE', *, *, #1092, .F. ) ;
#15374 = ORIENTED_EDGE ( 'NONE', *, *, #3418, .F. ) ;
#15375 = LINE ( 'NONE', #4699, #11890 ) ;
#15376 = DIRECTION ( 'NONE',  ( -0.000000000000000000, -1.000000000000000000, -0.000000000000000000 ) ) ;
#15377 = CIRCLE ( 'NONE', #10015, 1.599999999999997202 ) ;
#15378 = ADVANCED_FACE ( 'NONE', ( #17789 ), #1214, .T. ) ;
#15379 = LINE ( 'NONE', #18425, #15005 ) ;
#15380 = FACE_OUTER_BOUND ( 'NONE', #14901, .T. ) ;
#15381 = EDGE_CURVE ( 'NONE', #2609, #12636, #17593, .T. ) ;
#15382 = VECTOR ( 'NONE', #10635, 1000.000000000000000 ) ;
#15383 = CARTESIAN_POINT ( 'NONE',  ( -0.8561741729129461742, 66.06698729999999387, 45.60000000109246088 ) ) ;
#15384 = DIRECTION ( 'NONE',  ( -1.000000000000000000, 0.000000000000000000, 0.000000000000000000 ) ) ;
#15385 = AXIS2_PLACEMENT_3D ( 'NONE', #1459, #10155, #14886 ) ;
#15386 = CARTESIAN_POINT ( 'NONE',  ( -2.499999999999996003, 62.96446609406726225, 45.35000000218493454 ) ) ;
#15387 = ORIENTED_EDGE ( 'NONE', *, *, #18853, .T. ) ;
#15388 = EDGE_CURVE ( 'NONE', #12747, #17810, #12971, .T. ) ;
#15390 = ORIENTED_EDGE ( 'NONE', *, *, #2810, .F. ) ;
#15389 = ORIENTED_EDGE ( 'NONE', *, *, #18034, .F. ) ;
#15391 = CARTESIAN_POINT ( 'NONE',  ( -21.14459132904236327, -27.35725562635143149, 28.76367750791696309 ) ) ;
#15392 = AXIS2_PLACEMENT_3D ( 'NONE', #18527, #13805, #475 ) ;
#15393 = ORIENTED_EDGE ( 'NONE', *, *, #10084, .T. ) ;
#15394 = EDGE_LOOP ( 'NONE', ( #5584, #19027, #2738, #18749, #5074, #142, #9638, #4686, #18818, #6687, #10447, #17616, #84, #2947, #2741, #715 ) ) ;
#15395 = CARTESIAN_POINT ( 'NONE',  ( -17.51566270880199738, -25.64274437364856496, 35.98632249208304756 ) ) ;
#15396 = CARTESIAN_POINT ( 'NONE',  ( -11.64274437364854187, -30.14459132904234195, 11.70117750791695777 ) ) ;
#15397 = CARTESIAN_POINT ( 'NONE',  ( -1.265664690411616068E-16, 66.06698730000000808, 46.95000000109246940 ) ) ;
#15398 = CARTESIAN_POINT ( 'NONE',  ( -10.00000000000000000, -32.00000000000000711, 1.500000000000000000 ) ) ;
#15399 = ORIENTED_EDGE ( 'NONE', *, *, #16596, .F. ) ;
#15400 = CARTESIAN_POINT ( 'NONE',  ( -13.35725562635142794, -21.48433729119796709, 9.951177507916961318 ) ) ;
#15401 = CARTESIAN_POINT ( 'NONE',  ( -25.00000000000001421, -6.000000000000000000, 42.49999999999997868 ) ) ;
#15402 = ORIENTED_EDGE ( 'NONE', *, *, #9278, .T. ) ;
#15403 = EDGE_CURVE ( 'NONE', #13814, #11652, #11497, .T. ) ;
#15404 = EDGE_CURVE ( 'NONE', #17053, #14478, #11796, .T. ) ;
#15405 = CARTESIAN_POINT ( 'NONE',  ( -3.065533689247737392, -46.96461745799954457, 3.000000000000000000 ) ) ;
#15406 = ORIENTED_EDGE ( 'NONE', *, *, #12471, .T. ) ;
#15407 = FACE_OUTER_BOUND ( 'NONE', #1441, .T. ) ;
#15408 = FACE_OUTER_BOUND ( 'NONE', #10879, .T. ) ;
#15409 = CARTESIAN_POINT ( 'NONE',  ( -21.50000000000000000, 2.999000000000001442, 32.50000000000000000 ) ) ;
#15410 = CARTESIAN_POINT ( 'NONE',  ( -41.00000000000000711, 110.0000000000000000, 6.999999999999999112 ) ) ;
#15411 = DIRECTION ( 'NONE',  ( 0.000000000000000000, 0.000000000000000000, 1.000000000000000000 ) ) ;
#15412 = CARTESIAN_POINT ( 'NONE',  ( -2.066987300000001415, 63.14382582708705627, 48.80000000109247082 ) ) ;
#15413 = VECTOR ( 'NONE', #10735, 1000.000000000000000 ) ;
#15414 = EDGE_CURVE ( 'NONE', #13282, #6823, #11694, .T. ) ;
#15415 = CARTESIAN_POINT ( 'NONE',  ( -41.00000000000000711, 53.00000000000000711, -11.50000000000000000 ) ) ;
#15416 = DIRECTION ( 'NONE',  ( 1.000000000000000000, 0.000000000000000000, 0.000000000000000000 ) ) ;
#15417 = SHAPE_REPRESENTATION ( 'electro magnet', ( #1791 ), #11098 ) ;
#15418 = VECTOR ( 'NONE', #9172, 1000.000000000000000 ) ;
#15419 = DIRECTION ( 'NONE',  ( -0.000000000000000000, -0.000000000000000000, -1.000000000000000000 ) ) ;
#15420 = DIRECTION ( 'NONE',  ( 0.000000000000000000, 1.000000000000000000, -1.287488025362403787E-15 ) ) ;
#15421 = EDGE_LOOP ( 'NONE', ( #12937, #18442, #16032, #7147 ) ) ;
#15422 = CARTESIAN_POINT ( 'NONE',  ( -10.58745947852649927, -21.64274437364853654, 26.13867750791695599 ) ) ;
#15423 = PLANE ( 'NONE',  #1465 ) ;
#15424 = ORIENTED_EDGE ( 'NONE', *, *, #13973, .T. ) ;
#15425 = CARTESIAN_POINT ( 'NONE',  ( -9.955834737091903364, -25.17491895705294880, 18.26757249208304401 ) ) ;
#15426 = EDGE_CURVE ( 'NONE', #9967, #3232, #10514, .T. ) ;
#15427 = CARTESIAN_POINT ( 'NONE',  ( -17.68048971390462754, -22.64274437364856496, 15.86132249208304401 ) ) ;
#15428 = CARTESIAN_POINT ( 'NONE',  ( -10.00000000000000000, 47.00000000000000711, 30.00000000000000000 ) ) ;
#15429 = ORIENTED_EDGE ( 'NONE', *, *, #7438, .F. ) ;
#15430 = DIRECTION ( 'NONE',  ( -0.000000000000000000, -0.7071067811865493491, 0.7071067811865456854 ) ) ;
#15431 = ORIENTED_EDGE ( 'NONE', *, *, #64, .F. ) ;
#15432 = DIRECTION ( 'NONE',  ( 0.000000000000000000, -0.000000000000000000, 1.000000000000000000 ) ) ;
#15433 = DIRECTION ( 'NONE',  ( 1.000000000000000000, 0.000000000000000000, 0.000000000000000000 ) ) ;
#15434 = LINE ( 'NONE', #1906, #17563 ) ;
#15435 = CARTESIAN_POINT ( 'NONE',  ( -2.066987300000001415, 64.00000000000000000, 44.95000000109246940 ) ) ;
#15436 = CARTESIAN_POINT ( 'NONE',  ( 4.189607678530287593, 32.40336399182262284, 53.72836399182268252 ) ) ;
#15437 = LINE ( 'NONE', #9339, #10031 ) ;
#15438 = PLANE ( 'NONE',  #7391 ) ;
#15439 = ORIENTED_EDGE ( 'NONE', *, *, #14558, .F. ) ;
#15440 = CARTESIAN_POINT ( 'NONE',  ( -10.04416526290807710, -25.50457296725819489, 21.54492750791695599 ) ) ;
#15441 = CARTESIAN_POINT ( 'NONE',  ( 1.035533905932738197, 66.50000000000000000, 45.05000000218494449 ) ) ;
#15442 = CARTESIAN_POINT ( 'NONE',  ( -10.04416526290808953, -22.49542703274172695, 23.08007249208303335 ) ) ;
#15443 = CARTESIAN_POINT ( 'NONE',  ( -41.00000000000000000, 52.00000000000000711, -50.00000000000000000 ) ) ;
#15444 = CARTESIAN_POINT ( 'NONE',  ( -18.78091578003889950, -27.53959229564985378, 12.79492750791695421 ) ) ;
#15445 = CARTESIAN_POINT ( 'NONE',  ( -41.00000000000000711, 53.00000000000000711, -30.99999999999999645 ) ) ;
#15446 = CARTESIAN_POINT ( 'NONE',  ( -19.99999999999999645, -23.83517299489738051, 23.95117750791695954 ) ) ;
#15447 = CARTESIAN_POINT ( 'NONE',  ( 44.99999999999997158, -1.285879139104706187E-16, 53.40000000000000568 ) ) ;
#15448 = CARTESIAN_POINT ( 'NONE',  ( -16.17491895705296656, -29.04416526290807354, 30.08007249208304401 ) ) ;
#15449 = CARTESIAN_POINT ( 'NONE',  ( 0.8561741729129460632, 66.06698729999999387, 47.10000000109246798 ) ) ;
#15450 = CARTESIAN_POINT ( 'NONE',  ( 4.592425496802577917E-16, 61.50000000000000000, 49.39999999999999147 ) ) ;
#15451 = CARTESIAN_POINT ( 'NONE',  ( -14.99999999999999645, 73.00000000000001421, 26.99999999999997868 ) ) ;
#15452 = CARTESIAN_POINT ( 'NONE',  ( 37.49999999999999289, 0.000000000000000000, -25.00000000000001421 ) ) ;
#15453 = CARTESIAN_POINT ( 'NONE',  ( -1.461580736456473462, 62.53841926354353120, 49.05000000109247082 ) ) ;
#15454 = LINE ( 'NONE', #9178, #16131 ) ;
#15455 = ORIENTED_EDGE ( 'NONE', *, *, #16839, .F. ) ;
#15456 = ORIENTED_EDGE ( 'NONE', *, *, #9858, .T. ) ;
#15457 = CARTESIAN_POINT ( 'NONE',  ( -20.00369391078757886, -29.24501739517668142, 25.26757249208304401 ) ) ;
#15458 = CARTESIAN_POINT ( 'NONE',  ( -17.35725562635140307, -28.41254052147349185, 9.298822492083040459 ) ) ;
#15459 = ORIENTED_EDGE ( 'NONE', *, *, #12894, .F. ) ;
#15460 = CARTESIAN_POINT ( 'NONE',  ( -17.07549068051210739, -21.68318583509881847, 24.60742750791696309 ) ) ;
#15461 =( REPRESENTATION_RELATIONSHIP ('NONE','NONE', #7912, #15908 ) REPRESENTATION_RELATIONSHIP_WITH_TRANSFORMATION ( #13836 )SHAPE_REPRESENTATION_RELATIONSHIP( ) );
#15462 = CARTESIAN_POINT ( 'NONE',  ( 0.000000000000000000, 0.000000000000000000, 2.600000000000000089 ) ) ;
#15463 = CARTESIAN_POINT ( 'NONE',  ( -17.04047135212050890, -17.04416526290807710, 16.51757249208304046 ) ) ;
#15464 = CARTESIAN_POINT ( 'NONE',  ( -1.461580736456473462, 62.53841926354353120, 44.85000000109246798 ) ) ;
#15465 = CARTESIAN_POINT ( 'NONE',  ( 0.8561741729129460632, 66.06698729999999387, 46.10000000109246798 ) ) ;
#15466 = VERTEX_POINT ( 'NONE', #2781 ) ;
#15467 = ORIENTED_EDGE ( 'NONE', *, *, #14027, .F. ) ;
#15468 = EDGE_CURVE ( 'NONE', #16704, #291, #8759, .T. ) ;
#15469 = FACE_OUTER_BOUND ( 'NONE', #5376, .T. ) ;
#15470 = CARTESIAN_POINT ( 'NONE',  ( -44.99999999999998579, -1.285879139104706187E-16, -55.00000000000000000 ) ) ;
#15471 = CARTESIAN_POINT ( 'NONE',  ( 2.066987300000001415, 64.00000000000000000, 48.35000000109246798 ) ) ;
#15472 = CARTESIAN_POINT ( 'NONE',  ( -25.00000000000000711, -6.000000000000000000, -47.50000000000002132 ) ) ;
#15473 = EDGE_CURVE ( 'NONE', #16010, #12630, #8958, .T. ) ;
#15474 = CARTESIAN_POINT ( 'NONE',  ( -37.50000000000002132, 107.3545527679194436, 24.99999999999998224 ) ) ;
#15475 = VECTOR ( 'NONE', #9632, 1000.000000000000114 ) ;
#15476 = CARTESIAN_POINT ( 'NONE',  ( -1.040834085586084257E-14, 29.74264068711925901, 56.74264068711929809 ) ) ;
#15477 = EDGE_CURVE ( 'NONE', #428, #17877, #16145, .T. ) ;
#15478 = DIRECTION ( 'NONE',  ( -0.000000000000000000, 1.000000000000000000, -0.000000000000000000 ) ) ;
#15479 = ORIENTED_EDGE ( 'NONE', *, *, #14542, .T. ) ;
#15480 = ORIENTED_EDGE ( 'NONE', *, *, #5527, .T. ) ;
#15481 = CARTESIAN_POINT ( 'NONE',  ( -13.28918265808472299, -31.04416526290805933, 27.66992750791695954 ) ) ;
#15482 = ITEM_DEFINED_TRANSFORMATION ( 'NONE', 'NONE', #19262,  #1791 ) ;
#15483 = ORIENTED_EDGE ( 'NONE', *, *, #11511, .F. ) ;
#15484 = ORIENTED_EDGE ( 'NONE', *, *, #8780, .F. ) ;
#15485 = CARTESIAN_POINT ( 'NONE',  ( -17.31681416490117087, -21.92450931948788551, 37.08007249208304756 ) ) ;
#15486 = CARTESIAN_POINT ( 'NONE',  ( -9.020235676060220698, -27.64274437364852588, 11.26367750791695599 ) ) ;
#15487 =( GEOMETRIC_REPRESENTATION_CONTEXT ( 3 ) GLOBAL_UNCERTAINTY_ASSIGNED_CONTEXT ( ( #1794 ) ) GLOBAL_UNIT_ASSIGNED_CONTEXT ( ( #15170, #7722, #15364 ) ) REPRESENTATION_CONTEXT ( 'NONE', 'WORKASPACE' ) );
#15488 = VECTOR ( 'NONE', #16205, 1000.000000000000000 ) ;
#15489 = CARTESIAN_POINT ( 'NONE',  ( -1.265664690411616068E-16, 66.06698730000000808, 48.55000000109247082 ) ) ;
#15490 = DIRECTION ( 'NONE',  ( 0.000000000000000000, 0.000000000000000000, -1.000000000000000000 ) ) ;
#15491 = ORIENTED_EDGE ( 'NONE', *, *, #4085, .F. ) ;
#15492 = CARTESIAN_POINT ( 'NONE',  ( -17.07549068051210739, -21.68318583509881847, 29.85742750791696309 ) ) ;
#15493 = EDGE_CURVE ( 'NONE', #4727, #8108, #5539, .T. ) ;
#15494 = EDGE_LOOP ( 'NONE', ( #5658, #8244, #18925 ) ) ;
#15495 = DIRECTION ( 'NONE',  ( 1.156482317317871725E-16, 0.000000000000000000, -1.000000000000000000 ) ) ;
#15496 = ORIENTED_EDGE ( 'NONE', *, *, #1617, .F. ) ;
#15497 = DIRECTION ( 'NONE',  ( -0.000000000000000000, -1.000000000000000000, -0.000000000000000000 ) ) ;
#15498 = CARTESIAN_POINT ( 'NONE',  ( 1.300000000000000044, 1.478016689125442484, -1.626303258728256651E-15 ) ) ;
#15499 = DIRECTION ( 'NONE',  ( 0.7071067811865389130, -0.5000000000000073275, 0.5000000000000048850 ) ) ;
#15500 = CARTESIAN_POINT ( 'NONE',  ( -24.00000000000000711, 53.00000000000000711, 13.50000000000000000 ) ) ;
#15501 = CARTESIAN_POINT ( 'NONE',  ( -24.00000000000000000, 53.00000000000000711, 30.00000000000000000 ) ) ;
#15502 = CARTESIAN_POINT ( 'NONE',  ( 34.99999999999999289, -6.000000000000000000, 47.49999999999997868 ) ) ;
#15503 = PLANE ( 'NONE',  #12215 ) ;
#15504 = AXIS2_PLACEMENT_3D ( 'NONE', #6227, #10722, #3378 ) ;
#15505 = CARTESIAN_POINT ( 'NONE',  ( -3.400000000000017675, 29.65425233947097183, 56.47747564417432642 ) ) ;
#15506 = CIRCLE ( 'NONE', #12677, 1.500000000000001332 ) ;
#15507 = DIRECTION ( 'NONE',  ( -1.000000000000000000, 0.000000000000000000, 0.000000000000000000 ) ) ;
#15508 = ORIENTED_EDGE ( 'NONE', *, *, #4849, .T. ) ;
#15509 = CARTESIAN_POINT ( 'NONE',  ( -19.99999999999999645, -23.83517299489738051, 29.20117750791695599 ) ) ;
#15510 = DIRECTION ( 'NONE',  ( -0.000000000000000000, 0.000000000000000000, 1.000000000000000000 ) ) ;
#15511 = EDGE_CURVE ( 'NONE', #5957, #2980, #13065, .T. ) ;
#15512 = ORIENTED_EDGE ( 'NONE', *, *, #13926, .F. ) ;
#15513 = EDGE_CURVE ( 'NONE', #18191, #14223, #11596, .T. ) ;
#15514 = CARTESIAN_POINT ( 'NONE',  ( -16.17491895705296656, -29.04416526290807710, 35.33007249208301914 ) ) ;
#15515 = EDGE_CURVE ( 'NONE', #7101, #232, #1910, .T. ) ;
#15516 = CARTESIAN_POINT ( 'NONE',  ( -11.99999999999999289, -23.83517299489735564, 39.04882249208304756 ) ) ;
#15517 = VECTOR ( 'NONE', #1167, 1000.000000000000000 ) ;
#15518 = CARTESIAN_POINT ( 'NONE',  ( -40.00000000000000000, 53.00000000000000711, -12.50000000000000000 ) ) ;
#15519 = VERTEX_POINT ( 'NONE', #9448 ) ;
#15520 = AXIS2_PLACEMENT_3D ( 'NONE', #14517, #4231, #11667 ) ;
#15521 = DIRECTION ( 'NONE',  ( 1.000000000000000000, 0.000000000000000000, 0.000000000000000000 ) ) ;
#15522 = ORIENTED_EDGE ( 'NONE', *, *, #6386, .T. ) ;
#15523 = DIRECTION ( 'NONE',  ( 0.000000000000000000, 1.000000000000000000, -1.026972870230479989E-15 ) ) ;
#15524 = DIRECTION ( 'NONE',  ( 0.000000000000000000, 1.000000000000000000, 0.000000000000000000 ) ) ;
#15525 =( BOUNDED_CURVE ( )  B_SPLINE_CURVE ( 2, ( #316, #16489, #8931, #16786, #16390, #2953, #4638, #1494, #1687 ),
 .UNSPECIFIED., .F., .F. ) 
 B_SPLINE_CURVE_WITH_KNOTS ( ( 3, 2, 2, 2, 3 ),
 ( 0.4999999999999999445, 0.5178571428571427937, 0.5357142857142855874, 0.5535714285714283811, 0.5714285714285711748 ),
 .UNSPECIFIED. ) 
 CURVE ( )  GEOMETRIC_REPRESENTATION_ITEM ( )  RATIONAL_B_SPLINE_CURVE ( ( 1.000000000000000222, 0.9238795325112865164, 1.000000000000000000, 0.9238795325112867385, 1.000000000000000000, 0.9238795325112867385, 1.000000000000000000, 0.9238795325112877377, 0.9999999999999990008 ) ) 
 REPRESENTATION_ITEM ( '' )  );
#15526 = LINE ( 'NONE', #6611, #3799 ) ;
#15527 = FACE_BOUND ( 'NONE', #12241, .T. ) ;
#15528 = EDGE_CURVE ( 'NONE', #16168, #6563, #9158, .T. ) ;
#15529 =( NAMED_UNIT ( * ) SI_UNIT ( $, .STERADIAN. ) SOLID_ANGLE_UNIT ( ) );
#15530 = ADVANCED_FACE ( 'NONE', ( #18387 ), #46, .F. ) ;
#15531 = CARTESIAN_POINT ( 'NONE',  ( -32.50000000000000000, 52.00000000000000711, -35.00000000000000000 ) ) ;
#15532 = VECTOR ( 'NONE', #8311, 1000.000000000000000 ) ;
#15533 = DIRECTION ( 'NONE',  ( -1.156482317317871478E-16, 1.000000000000000000, 0.000000000000000000 ) ) ;
#15534 = VECTOR ( 'NONE', #10848, 1000.000000000000000 ) ;
#15535 = VERTEX_POINT ( 'NONE', #9340 ) ;
#15536 = CARTESIAN_POINT ( 'NONE',  ( -19.24771351637089367, -21.35725562635142438, 29.63867750791695599 ) ) ;
#15537 = CARTESIAN_POINT ( 'NONE',  ( -1.035533905932738863, 61.50000000000000000, 44.65000000218494591 ) ) ;
#15538 = CARTESIAN_POINT ( 'NONE',  ( -16.50457296725825174, -19.04416526290807354, 16.51757249208304046 ) ) ;
#15539 = CARTESIAN_POINT ( 'NONE',  ( -44.99999999999998579, 6.000000000000000000, -55.00000000000000000 ) ) ;
#15540 = CARTESIAN_POINT ( 'NONE',  ( -12.64274437364855252, -28.41254052147347053, 22.20117750791695599 ) ) ;
#15541 = CARTESIAN_POINT ( 'NONE',  ( 1.753982408753060218, -46.96461745799954457, 1.500000000000000000 ) ) ;
#15542 = AXIS2_PLACEMENT_3D ( 'NONE', #12168, #121, #13341 ) ;
#15543 = CARTESIAN_POINT ( 'NONE',  ( -9.955834737091912245, -22.82508104294696238, 31.60742750791695954 ) ) ;
#15544 = CARTESIAN_POINT ( 'NONE',  ( 1.035533905932739751, 61.50000000000000000, 47.04999999999999716 ) ) ;
#15545 = CARTESIAN_POINT ( 'NONE',  ( -16.17491895705296656, -29.04416526290807354, 24.83007249208304401 ) ) ;
#15546 = VECTOR ( 'NONE', #15645, 1000.000000000000000 ) ;
#15547 = CARTESIAN_POINT ( 'NONE',  ( 2.500000000000001776, 64.00000000000000000, 49.60000000000000142 ) ) ;
#15548 = DIRECTION ( 'NONE',  ( 0.000000000000000000, 0.000000000000000000, -1.000000000000000000 ) ) ;
#15549 = LINE ( 'NONE', #2119, #11946 ) ;
#15550 = EDGE_CURVE ( 'NONE', #11173, #5104, #3376, .T. ) ;
#15551 = CARTESIAN_POINT ( 'NONE',  ( -1.035533905932738641, 66.50000000000000000, 48.35000000218494165 ) ) ;
#15552 = CARTESIAN_POINT ( 'NONE',  ( 2.066987300000002303, 63.14382582708705627, 46.90000000109247225 ) ) ;
#15553 = CARTESIAN_POINT ( 'NONE',  ( -7.499999999999994671, -38.00000000000000000, 12.50000000000000000 ) ) ;
#15554 = ORIENTED_EDGE ( 'NONE', *, *, #4900, .T. ) ;
#15555 = CARTESIAN_POINT ( 'NONE',  ( -11.64274437364859693, -17.85540867095757989, 27.67382249208304401 ) ) ;
#15556 = PRESENTATION_LAYER_ASSIGNMENT (  '', '', ( #12096 ) ) ;
#15557 = VECTOR ( 'NONE', #9421, 1000.000000000000000 ) ;
#15558 = CARTESIAN_POINT ( 'NONE',  ( -9.999999999999994671, -23.83517299489734143, 7.548822492083041347 ) ) ;
#15559 = CARTESIAN_POINT ( 'NONE',  ( -17.95583473709191580, -23.03132541760400898, 34.66992750791696665 ) ) ;
#15560 = DIRECTION ( 'NONE',  ( 0.000000000000000000, -1.000000000000000000, -0.000000000000000000 ) ) ;
#15561 = CARTESIAN_POINT ( 'NONE',  ( -9.020235676060250896, -20.35725562635137820, 22.86132249208304046 ) ) ;
#15562 = CARTESIAN_POINT ( 'NONE',  ( -2.066987300000001415, 64.00000000000000000, 46.35000000109246798 ) ) ;
#15563 = DIRECTION ( 'NONE',  ( 0.000000000000000000, 0.000000000000000000, 1.000000000000000000 ) ) ;
#15564 = VERTEX_POINT ( 'NONE', #438 ) ;
#15565 = VERTEX_POINT ( 'NONE', #1709 ) ;
#15566 = CARTESIAN_POINT ( 'NONE',  ( -1.265664690411616068E-16, 66.06698730000000808, 44.55000000109247082 ) ) ;
#15567 = LINE ( 'NONE', #12328, #3177 ) ;
#15568 = CARTESIAN_POINT ( 'NONE',  ( 14.99999999999998579, 52.00000000000000711, 26.99999999999997158 ) ) ;
#15569 = DIRECTION ( 'NONE',  ( -1.000000000000000000, -0.000000000000000000, -0.000000000000000000 ) ) ;
#15570 = AXIS2_PLACEMENT_3D ( 'NONE', #1374, #11651, #3033 ) ;
#15571 = DIRECTION ( 'NONE',  ( 0.000000000000000000, 0.000000000000000000, -1.000000000000000000 ) ) ;
#15572 = ADVANCED_FACE ( 'NONE', ( #1520 ), #16514, .T. ) ;
#15573 = CARTESIAN_POINT ( 'NONE',  ( 32.50000000000000000, 52.00000000000000711, -32.50000000000000000 ) ) ;
#15574 = CARTESIAN_POINT ( 'NONE',  ( -1.767766952966369765, 62.23223304703363112, 47.69999999999999574 ) ) ;
#15575 = ORIENTED_EDGE ( 'NONE', *, *, #1702, .T. ) ;
#15576 = EDGE_LOOP ( 'NONE', ( #9772, #12532, #13353, #18562 ) ) ;
#15577 = CARTESIAN_POINT ( 'NONE',  ( -12.95952864787955150, -17.04416526290805933, 25.48242750791696309 ) ) ;
#15578 = VERTEX_POINT ( 'NONE', #6422 ) ;
#15580 = ORIENTED_EDGE ( 'NONE', *, *, #1658, .F. ) ;
#15579 = ORIENTED_EDGE ( 'NONE', *, *, #6499, .T. ) ;
#15581 = CARTESIAN_POINT ( 'NONE',  ( -12.04416526290808420, -23.03132541760398766, 33.58007249208304756 ) ) ;
#15582 = CARTESIAN_POINT ( 'NONE',  ( -9.996306089212364299, -29.24501739517662813, 16.73242750791695954 ) ) ;
#15583 = CARTESIAN_POINT ( 'NONE',  ( -2.500000000000003997, 65.03553390593273775, 47.55000000000000426 ) ) ;
#15584 = CARTESIAN_POINT ( 'NONE',  ( 4.592425496802577917E-16, 61.50000000000000000, 48.70000000218494307 ) ) ;
#15585 = DIRECTION ( 'NONE',  ( -1.734723475976807094E-15, 1.000000000000000000, 0.000000000000000000 ) ) ;
#15586 = ORIENTED_EDGE ( 'NONE', *, *, #4764, .T. ) ;
#15587 = CARTESIAN_POINT ( 'NONE',  ( -17.99999999999999645, -23.83517299489736985, 23.95117750791696309 ) ) ;
#15588 = FILL_AREA_STYLE_COLOUR ( '', #12558 ) ;
#15589 = VERTEX_POINT ( 'NONE', #1622 ) ;
#15590 = CARTESIAN_POINT ( 'NONE',  ( 0.1249999999999895917, 29.74264068711926257, 56.74264068711929809 ) ) ;
#15591 = VERTEX_POINT ( 'NONE', #9056 ) ;
#15592 = CARTESIAN_POINT ( 'NONE',  ( 1.000000000000000222, -28.00000000000000000, 9.500000000000001776 ) ) ;
#15593 = DIRECTION ( 'NONE',  ( -0.000000000000000000, 0.000000000000000000, 1.000000000000000000 ) ) ;
#15594 = LINE ( 'NONE', #11733, #2797 ) ;
#15595 = CARTESIAN_POINT ( 'NONE',  ( 2.066987300000002303, 63.14382582708705627, 47.50000000109246656 ) ) ;
#15596 = CARTESIAN_POINT ( 'NONE',  ( -0.8561741729129461742, 66.06698730000000808, 47.20000000109246940 ) ) ;
#15597 = DIRECTION ( 'NONE',  ( -1.000000000000000000, -0.000000000000000000, -0.000000000000000000 ) ) ;
#15598 = CARTESIAN_POINT ( 'NONE',  ( -24.00000000000000000, 53.00000000000000711, -37.50000000000000711 ) ) ;
#15599 = CARTESIAN_POINT ( 'NONE',  ( 14.33926609531033058, -43.78611686177728046, 3.000000000000000000 ) ) ;
#15600 = VERTEX_POINT ( 'NONE', #13657 ) ;
#15601 = EDGE_CURVE ( 'NONE', #12045, #4427, #13015, .T. ) ;
#15603 = EDGE_CURVE ( 'NONE', #16897, #16279, #18289, .T. ) ;
#15602 = CARTESIAN_POINT ( 'NONE',  ( -11.46040770435012668, -27.78091578003887463, 27.23242750791694888 ) ) ;
#15604 = DIRECTION ( 'NONE',  ( 0.000000000000000000, -0.7071067811865455743, -0.7071067811865495711 ) ) ;
#15605 = VERTEX_POINT ( 'NONE', #10518 ) ;
#15606 = CARTESIAN_POINT ( 'NONE',  ( -13.49542703274174116, -28.95583473709188738, 29.64257249208303691 ) ) ;
#15607 = CARTESIAN_POINT ( 'NONE',  ( -17.99999999999999645, -24.16482700510260173, 36.42382249208304756 ) ) ;
#15608 = SURFACE_STYLE_FILL_AREA ( #610 ) ;
#15609 = EDGE_LOOP ( 'NONE', ( #18621, #10305, #11350, #15424 ) ) ;
#15610 = CARTESIAN_POINT ( 'NONE',  ( -50.00000000000002132, 115.0000000000000000, 37.49999999999997868 ) ) ;
#15611 = ORIENTED_EDGE ( 'NONE', *, *, #9348, .T. ) ;
#15612 = CARTESIAN_POINT ( 'NONE',  ( 1.035533905932738197, 66.50000000000000000, 45.05000000218493739 ) ) ;
#15613 = DIRECTION ( 'NONE',  ( -0.000000000000000000, -0.7071067811865456854, -0.7071067811865494601 ) ) ;
#15614 = VECTOR ( 'NONE', #1929, 1000.000000000000000 ) ;
#15615 = CARTESIAN_POINT ( 'NONE',  ( 1.300000000000000044, 1.478016689125442484, -1.626303258728256651E-15 ) ) ;
#15616 = ADVANCED_FACE ( 'NONE', ( #6224 ), #10911, .T. ) ;
#15617 = EDGE_CURVE ( 'NONE', #12352, #15030, #7488, .T. ) ;
#15618 = CARTESIAN_POINT ( 'NONE',  ( -32.50000000000000000, 53.00000000000000711, 17.64999999999999147 ) ) ;
#15619 = PLANE ( 'NONE',  #7235 ) ;
#15620 = FACE_OUTER_BOUND ( 'NONE', #9197, .T. ) ;
#15621 = VECTOR ( 'NONE', #1844, 1000.000000000000000 ) ;
#15622 = CARTESIAN_POINT ( 'NONE',  ( 0.000000000000000000, 64.00000000000000000, 49.99999999999999289 ) ) ;
#15623 = ORIENTED_EDGE ( 'NONE', *, *, #15148, .T. ) ;
#15624 = AXIS2_PLACEMENT_3D ( 'NONE', #12494, #1724, #1823 ) ;
#15625 = CARTESIAN_POINT ( 'NONE',  ( -19.99999999999999645, -23.83517299489738051, 29.20117750791695599 ) ) ;
#15626 = CARTESIAN_POINT ( 'NONE',  ( 2.500000000000001776, 64.00000000000000000, 44.90000000218493881 ) ) ;
#15627 = CARTESIAN_POINT ( 'NONE',  ( -9.955834737091903364, -25.17491895705294880, 34.01757249208303335 ) ) ;
#15628 =( BOUNDED_CURVE ( )  B_SPLINE_CURVE ( 2, ( #13321, #105, #296, #5991, #4522, #10480, #10278, #16473, #18050 ),
 .UNSPECIFIED., .F., .F. ) 
 B_SPLINE_CURVE_WITH_KNOTS ( ( 3, 2, 2, 2, 3 ),
 ( 0.3571428571428571508, 0.3750000000000000000, 0.3928571428571427937, 0.4107142857142855874, 0.4285714285714284366 ),
 .UNSPECIFIED. ) 
 CURVE ( )  GEOMETRIC_REPRESENTATION_ITEM ( )  RATIONAL_B_SPLINE_CURVE ( ( 1.000000000000000000, 0.9238795325112867385, 1.000000000000000000, 0.9238795325112867385, 1.000000000000000000, 0.9238795325112867385, 1.000000000000000000, 0.9238795325112871826, 0.9999999999999995559 ) ) 
 REPRESENTATION_ITEM ( '' )  );
#15629 = CARTESIAN_POINT ( 'NONE',  ( -41.00000000000000711, 53.00000000000000711, -25.50000000000000000 ) ) ;
#15630 = CARTESIAN_POINT ( 'NONE',  ( -15.16482700510259640, -28.99999999999998224, 17.38867750791695599 ) ) ;
#15631 = DIRECTION ( 'NONE',  ( -0.000000000000000000, -1.000000000000000000, -0.000000000000000000 ) ) ;
#15633 = CARTESIAN_POINT ( 'NONE',  ( -11.46040770435012490, -27.78091578003888173, 37.73242750791695954 ) ) ;
#15632 = VECTOR ( 'NONE', #4306, 1000.000000000000000 ) ;
#15634 = CARTESIAN_POINT ( 'NONE',  ( -1.530808498934192803E-16, 66.50000000000000000, 46.70000000218494307 ) ) ;
#15635 = CARTESIAN_POINT ( 'NONE',  ( -9.955834737091903364, -25.17491895705295235, 23.51757249208304046 ) ) ;
#15636 = EDGE_CURVE ( 'NONE', #10068, #14997, #12295, .T. ) ;
#15637 = CARTESIAN_POINT ( 'NONE',  ( 1.035533905932738197, 66.50000000000000000, 49.75000000000000000 ) ) ;
#15638 = LINE ( 'NONE', #738, #11509 ) ;
#15640 = LINE ( 'NONE', #2211, #7247 ) ;
#15639 = AXIS2_PLACEMENT_3D ( 'NONE', #18277, #613, #12576 ) ;
#15641 = VECTOR ( 'NONE', #11140, 1000.000000000000000 ) ;
#15642 = CARTESIAN_POINT ( 'NONE',  ( 2.500000000000001776, 64.00000000000000000, 47.30000000218494449 ) ) ;
#15643 = EDGE_CURVE ( 'NONE', #7955, #12973, #16906, .T. ) ;
#15644 = CARTESIAN_POINT ( 'NONE',  ( -1.035533905932738641, 66.50000000000000000, 49.04999999999999716 ) ) ;
#15645 = DIRECTION ( 'NONE',  ( 1.000000000000000000, 0.000000000000000000, 0.000000000000000000 ) ) ;
#15646 = VERTEX_POINT ( 'NONE', #17984 ) ;
#15647 = CARTESIAN_POINT ( 'NONE',  ( -11.64274437364859693, -17.85540867095757989, 38.17382249208303335 ) ) ;
#15648 = CIRCLE ( 'NONE', #18167, 4.250000000000000000 ) ;
#15649 = SHAPE_REPRESENTATION_RELATIONSHIP ( 'NONE' , 'NONE' ,  #2502, #14596 ) ;
#15650 = CARTESIAN_POINT ( 'NONE',  ( 2.066987300000001415, 64.85617417291294373, 46.80000000109247082 ) ) ;
#15651 = CARTESIAN_POINT ( 'NONE',  ( -14.03132541760401786, -21.04416526290806289, 30.73242750791696309 ) ) ;
#15652 = CARTESIAN_POINT ( 'NONE',  ( -19.99999999999999645, -32.00000000000000711, 1.500000000000000000 ) ) ;
#15653 = CARTESIAN_POINT ( 'NONE',  ( -8.044165262908093084, -21.95952864787946979, 28.33007249208304756 ) ) ;
#15654 = AXIS2_PLACEMENT_3D ( 'NONE', #13131, #17653, #4228 ) ;
#15655 = CARTESIAN_POINT ( 'NONE',  ( -2.066987300000001859, 64.85617417291294373, 46.30000000109247082 ) ) ;
#15656 = ORIENTED_EDGE ( 'NONE', *, *, #1479, .T. ) ;
#15657 = EDGE_CURVE ( 'NONE', #5462, #4687, #12089, .T. ) ;
#15658 = ORIENTED_EDGE ( 'NONE', *, *, #1039, .T. ) ;
#15659 = CARTESIAN_POINT ( 'NONE',  ( 21.50000000000001421, 115.0000000000000000, 32.49999999999998579 ) ) ;
#15660 = CARTESIAN_POINT ( 'NONE',  ( 41.00000000000000000, 47.00000000000000711, -50.00000000000000000 ) ) ;
#15661 = VECTOR ( 'NONE', #1907, 1000.000000000000000 ) ;
#15662 = CARTESIAN_POINT ( 'NONE',  ( -0.8561741729129461742, 66.06698730000000808, 45.40000000109247225 ) ) ;
#15663 = FACE_OUTER_BOUND ( 'NONE', #4200, .T. ) ;
#15664 = CARTESIAN_POINT ( 'NONE',  ( 2.499999999999996891, 62.96446609406726225, 47.94999999999998863 ) ) ;
#15665 = VECTOR ( 'NONE', #15182, 1000.000000000000000 ) ;
#15666 = CARTESIAN_POINT ( 'NONE',  ( -41.00000000000000711, 110.0000000000000000, -5.000000000000000888 ) ) ;
#15667 = VECTOR ( 'NONE', #14689, 1000.000000000000000 ) ;
#15668 = DIRECTION ( 'NONE',  ( -0.000000000000000000, 0.7071067811865452413, 0.7071067811865497932 ) ) ;
#15669 = VERTEX_POINT ( 'NONE', #4560 ) ;
#15670 = ORIENTED_EDGE ( 'NONE', *, *, #14652, .F. ) ;
#15671 = PRODUCT_RELATED_PRODUCT_CATEGORY ( 'part', '', ( #8955 ) ) ;
#15672 = CARTESIAN_POINT ( 'NONE',  ( -18.35725562635144925, -17.85540867095761186, 30.07617750791695599 ) ) ;
#15673 = ORIENTED_EDGE ( 'NONE', *, *, #3882, .F. ) ;
#15674 = AXIS2_PLACEMENT_3D ( 'NONE', #4157, #11582, #14632 ) ;
#15676 = ORIENTED_EDGE ( 'NONE', *, *, #7869, .F. ) ;
#15675 = ORIENTED_EDGE ( 'NONE', *, *, #15747, .F. ) ;
#15677 = CARTESIAN_POINT ( 'NONE',  ( -12.04416526290808420, -23.03132541760398766, 28.33007249208304756 ) ) ;
#15678 = CARTESIAN_POINT ( 'NONE',  ( -12.95952864787955150, -17.04416526290805933, 14.98242750791695777 ) ) ;
#15679 = VECTOR ( 'NONE', #8885, 1000.000000000000000 ) ;
#15680 = DIRECTION ( 'NONE',  ( 1.000000000000000000, 0.000000000000000000, 0.000000000000000000 ) ) ;
#15681 = CARTESIAN_POINT ( 'NONE',  ( 4.592425496802577917E-16, 61.50000000000000000, 46.30000000218493739 ) ) ;
#15682 = DIRECTION ( 'NONE',  ( 0.000000000000000000, -1.000000000000000000, -0.000000000000000000 ) ) ;
#15683 = ORIENTED_EDGE ( 'NONE', *, *, #4947, .T. ) ;
#15684 = CARTESIAN_POINT ( 'NONE',  ( -17.99999999999999645, -23.83517299489736985, 29.20117750791695954 ) ) ;
#15685 = AXIS2_PLACEMENT_3D ( 'NONE', #12528, #12333, #18428 ) ;
#15686 = LINE ( 'NONE', #5390, #13792 ) ;
#15687 = ORIENTED_EDGE ( 'NONE', *, *, #5808, .F. ) ;
#15688 = PLANE ( 'NONE',  #9071 ) ;
#15689 = ORIENTED_EDGE ( 'NONE', *, *, #16114, .T. ) ;
#15690 = CARTESIAN_POINT ( 'NONE',  ( -15.20357423236093375, -43.78611686177728046, 3.000000000000000000 ) ) ;
#15691 = DIRECTION ( 'NONE',  ( -1.000000000000000000, 0.000000000000000000, -9.251858538542970348E-17 ) ) ;
#15692 = CARTESIAN_POINT ( 'NONE',  ( -40.00000000000000711, 110.0000000000000000, -25.49999999999999645 ) ) ;
#15693 = CARTESIAN_POINT ( 'NONE',  ( -2.066987300000001415, 63.14382582708705627, 47.20000000109248361 ) ) ;
#15694 = VECTOR ( 'NONE', #7430, 1000.000000000000000 ) ;
#15695 = CARTESIAN_POINT ( 'NONE',  ( -1.461580736456473906, 65.46158073645646880, 48.05000000109247082 ) ) ;
#15696 = LINE ( 'NONE', #2265, #7857 ) ;
#15697 = AXIS2_PLACEMENT_3D ( 'NONE', #13135, #12942, #19231 ) ;
#15698 = CARTESIAN_POINT ( 'NONE',  ( 2.499999999999992895, 65.03553390593273775, 49.64999999999998437 ) ) ;
#15699 = LINE ( 'NONE', #2268, #2665 ) ;
#15700 = ORIENTED_EDGE ( 'NONE', *, *, #15388, .T. ) ;
#15701 = ORIENTED_EDGE ( 'NONE', *, *, #18148, .F. ) ;
#15702 = CARTESIAN_POINT ( 'NONE',  ( -18.53959229564986799, -20.21908421996107563, 35.10742750791694533 ) ) ;
#15703 = VECTOR ( 'NONE', #4827, 1000.000000000000000 ) ;
#15704 = LINE ( 'NONE', #6780, #3024 ) ;
#15705 = ORIENTED_EDGE ( 'NONE', *, *, #6024, .T. ) ;
#15706 = CARTESIAN_POINT ( 'NONE',  ( -10.04416526290808953, -22.49542703274172695, 33.58007249208304046 ) ) ;
#15707 = VECTOR ( 'NONE', #1637, 1000.000000000000000 ) ;
#15708 = CARTESIAN_POINT ( 'NONE',  ( -1.767766952966370209, 65.76776695296638309, 45.89999999999999858 ) ) ;
#15709 = CARTESIAN_POINT ( 'NONE',  ( -16.64274437364858272, -21.48433729119797420, 26.79882249208304401 ) ) ;
#15710 = FACE_OUTER_BOUND ( 'NONE', #13583, .T. ) ;
#15711 = EDGE_LOOP ( 'NONE', ( #12439, #7516, #17722, #3617 ) ) ;
#15712 = AXIS2_PLACEMENT_3D ( 'NONE', #16731, #9270, #4234 ) ;
#15713 = DIRECTION ( 'NONE',  ( 1.000000000000000000, 0.000000000000000000, 0.000000000000000000 ) ) ;
#15714 = ORIENTED_EDGE ( 'NONE', *, *, #16344, .T. ) ;
#15715 = CARTESIAN_POINT ( 'NONE',  ( -9.551088096457694952E-15, 20.55025253169411670, 57.44974746830580870 ) ) ;
#15716 = EDGE_CURVE ( 'NONE', #6116, #10089, #18085, .T. ) ;
#15717 = ADVANCED_FACE ( 'NONE', ( #13758 ), #10811, .T. ) ;
#15718 = CYLINDRICAL_SURFACE ( 'NONE', #6114, 2.500000000000001776 ) ;
#15719 = VECTOR ( 'NONE', #5568, 1000.000000000000000 ) ;
#15720 = DIRECTION ( 'NONE',  ( -1.000000000000000000, -0.000000000000000000, -0.000000000000000000 ) ) ;
#15721 = EDGE_CURVE ( 'NONE', #10544, #1168, #7790, .T. ) ;
#15722 = FACE_BOUND ( 'NONE', #18139, .T. ) ;
#15723 =( REPRESENTATION_RELATIONSHIP ('NONE','NONE', #7912, #6533 ) REPRESENTATION_RELATIONSHIP_WITH_TRANSFORMATION ( #216 )SHAPE_REPRESENTATION_RELATIONSHIP( ) );
#15724 = FACE_OUTER_BOUND ( 'NONE', #3106, .T. ) ;
#15726 = ADVANCED_FACE ( 'NONE', ( #6798, #18756, #11103 ), #2002, .T. ) ;
#15725 = CARTESIAN_POINT ( 'NONE',  ( 32.49999999999998579, -6.000000000000000000, 24.99999999999998224 ) ) ;
#15727 = CARTESIAN_POINT ( 'NONE',  ( 3.999999999999998224, 67.00000000000000000, 30.00000000000000000 ) ) ;
#15728 = ORIENTED_EDGE ( 'NONE', *, *, #4571, .T. ) ;
#15729 = VECTOR ( 'NONE', #17108, 1000.000000000000000 ) ;
#15730 = CARTESIAN_POINT ( 'NONE',  ( -10.58745947852649927, -21.64274437364853654, 26.13867750791695599 ) ) ;
#15731 = CARTESIAN_POINT ( 'NONE',  ( 1.461580736456473684, 65.46158073645646880, 49.25000000109246656 ) ) ;
#15732 = EDGE_CURVE ( 'NONE', #3523, #10448, #5329, .T. ) ;
#15733 = CARTESIAN_POINT ( 'NONE',  ( -20.04416526290809131, -22.82508104294699791, 31.39257249208304046 ) ) ;
#15734 = CARTESIAN_POINT ( 'NONE',  ( -19.99999999999999645, -32.00000000000000711, 0.000000000000000000 ) ) ;
#15735 = CARTESIAN_POINT ( 'NONE',  ( -12.35725562635143682, -19.75228648362908501, 36.20117750791695954 ) ) ;
#15736 = PLANE ( 'NONE',  #17368 ) ;
#15737 = CARTESIAN_POINT ( 'NONE',  ( -17.64274437364855430, -28.24771351637087236, 38.82617750791695954 ) ) ;
#15738 = DIRECTION ( 'NONE',  ( -0.000000000000000000, -0.000000000000000000, -1.000000000000000000 ) ) ;
#15739 = CARTESIAN_POINT ( 'NONE',  ( -18.78091578003892792, -20.46040770435013556, 21.33007249208304046 ) ) ;
#15740 = CARTESIAN_POINT ( 'NONE',  ( 2.066987300000001859, 64.85617417291294373, 45.40000000109246514 ) ) ;
#15741 = CYLINDRICAL_SURFACE ( 'NONE', #12162, 1.500000000000001332 ) ;
#15742 = CARTESIAN_POINT ( 'NONE',  ( 5.799326430397230503, 29.83055285973283333, 56.65377616443626607 ) ) ;
#15743 = CARTESIAN_POINT ( 'NONE',  ( 1.767766952966370653, 62.23223304703363112, 49.49999999999999289 ) ) ;
#15744 = CARTESIAN_POINT ( 'NONE',  ( 32.50000000000000000, 52.00000000000000711, 17.49999999999999645 ) ) ;
#15745 = ORIENTED_EDGE ( 'NONE', *, *, #13350, .F. ) ;
#15746 = ITEM_DEFINED_TRANSFORMATION ( 'NONE', 'NONE', #15504,  #1791 ) ;
#15747 = EDGE_CURVE ( 'NONE', #11338, #1767, #17194, .T. ) ;
#15748 = CARTESIAN_POINT ( 'NONE',  ( -0.8561741729129466183, 61.93301270000000613, 45.70000000109248361 ) ) ;
#15749 = ADVANCED_FACE ( 'NONE', ( #15620 ), #14152, .T. ) ;
#15750 = CARTESIAN_POINT ( 'NONE',  ( -17.68048971390461688, -25.35725562635141372, 28.76367750791696309 ) ) ;
#15751 = CARTESIAN_POINT ( 'NONE',  ( -41.00000000000000000, 52.00000000000000711, 30.00000000000000000 ) ) ;
#15752 = EDGE_CURVE ( 'NONE', #3686, #18580, #9729, .T. ) ;
#15753 = CARTESIAN_POINT ( 'NONE',  ( -8.855408670957602979, -27.35725562635137820, 39.48632249208304046 ) ) ;
#15754 = CARTESIAN_POINT ( 'NONE',  ( -2.066987300000001415, 63.14382582708705627, 48.00000000109246656 ) ) ;
#15755 = ORIENTED_EDGE ( 'NONE', *, *, #12857, .T. ) ;
#15756 = EDGE_CURVE ( 'NONE', #9100, #677, #3666, .T. ) ;
#15757 = PLANE ( 'NONE',  #5639 ) ;
#15758 = CARTESIAN_POINT ( 'NONE',  ( 1.035533905932739751, 61.50000000000000000, 45.55000000218493739 ) ) ;
#15759 = CARTESIAN_POINT ( 'NONE',  ( -2.066987300000001415, 64.00000000000000000, 45.55000000109246372 ) ) ;
#15760 = CARTESIAN_POINT ( 'NONE',  ( -3.999999999999996447, 47.00000000000000711, 34.99999999999999289 ) ) ;
#15761 = CARTESIAN_POINT ( 'NONE',  ( -24.00000000000000000, 53.00000000000000711, 30.00000000000000000 ) ) ;
#15762 = DIRECTION ( 'NONE',  ( 0.000000000000000000, 0.000000000000000000, 1.000000000000000000 ) ) ;
#15763 = CARTESIAN_POINT ( 'NONE',  ( 1.035533905932739751, 61.50000000000000000, 47.85000000000000142 ) ) ;
#15764 = ADVANCED_FACE ( 'NONE', ( #18859 ), #12858, .F. ) ;
#15765 = ORIENTED_EDGE ( 'NONE', *, *, #11409, .T. ) ;
#15766 = ORIENTED_EDGE ( 'NONE', *, *, #18100, .F. ) ;
#15767 = ADVANCED_FACE ( 'NONE', ( #8088 ), #15438, .T. ) ;
#15768 = CARTESIAN_POINT ( 'NONE',  ( -20.24501739517664234, -29.00369391078761439, 39.04492750791695954 ) ) ;
#15769 = ORIENTED_EDGE ( 'NONE', *, *, #3099, .T. ) ;
#15771 = VERTEX_POINT ( 'NONE', #723 ) ;
#15770 = ORIENTED_EDGE ( 'NONE', *, *, #11308, .T. ) ;
#15772 = CARTESIAN_POINT ( 'NONE',  ( -15.16482700510262482, -20.99999999999997513, 27.23632249208304046 ) ) ;
#15773 = CARTESIAN_POINT ( 'NONE',  ( -21.99999999999999289, -23.83517299489739116, 29.20117750791695244 ) ) ;
#15774 = FACE_BOUND ( 'NONE', #14991, .T. ) ;
#15775 = CARTESIAN_POINT ( 'NONE',  ( -2.500000000000000888, 62.96446609406726935, 46.15000000218493881 ) ) ;
#15776 = FACE_OUTER_BOUND ( 'NONE', #2619, .T. ) ;
#15777 = EDGE_LOOP ( 'NONE', ( #6307, #13287, #1521, #9522 ) ) ;
#15778 = LINE ( 'NONE', #8327, #11912 ) ;
#15779 = ORIENTED_EDGE ( 'NONE', *, *, #16839, .T. ) ;
#15780 = DIRECTION ( 'NONE',  ( 0.000000000000000000, 0.000000000000000000, -1.000000000000000000 ) ) ;
#15781 = VERTEX_POINT ( 'NONE', #17287 ) ;
#15782 = DIRECTION ( 'NONE',  ( -1.156482317317871478E-16, 1.000000000000000000, 0.000000000000000000 ) ) ;
#15783 = PRODUCT_DEFINITION ( 'UNKNOWN', '', #5174, #9431 ) ;
#15784 = DIRECTION ( 'NONE',  ( 0.000000000000000000, -0.7071067811865493491, 0.7071067811865456854 ) ) ;
#15785 = CARTESIAN_POINT ( 'NONE',  ( 8.000000000000014211, 60.00000000000001421, 66.99999999999997158 ) ) ;
#15786 = CARTESIAN_POINT ( 'NONE',  ( -1.461580736456473462, 62.53841926354353120, 45.65000000109247225 ) ) ;
#15787 = CARTESIAN_POINT ( 'NONE',  ( -1.461580736456473462, 62.53841926354353120, 49.05000000109247082 ) ) ;
#15788 = DIRECTION ( 'NONE',  ( 0.000000000000000000, 0.000000000000000000, 1.000000000000000000 ) ) ;
#15789 = LINE ( 'NONE', #15977, #13959 ) ;
#15790 = CARTESIAN_POINT ( 'NONE',  ( -0.1250000000000104083, 25.64142146683625612, 60.84290755733282197 ) ) ;
#15791 = EDGE_CURVE ( 'NONE', #13516, #3717, #7992, .T. ) ;
#15792 = ORIENTED_EDGE ( 'NONE', *, *, #18759, .T. ) ;
#15793 = ORIENTED_EDGE ( 'NONE', *, *, #14752, .T. ) ;
#15794 = CARTESIAN_POINT ( 'NONE',  ( -10.04416526290807710, -25.50457296725819489, 26.79492750791695954 ) ) ;
#15795 = DIRECTION ( 'NONE',  ( 0.000000000000000000, 0.000000000000000000, 1.000000000000000000 ) ) ;
#15796 = ORIENTED_EDGE ( 'NONE', *, *, #8394, .F. ) ;
#15797 = VECTOR ( 'NONE', #15809, 1000.000000000000114 ) ;
#15798 = CARTESIAN_POINT ( 'NONE',  ( -13.82508104294702100, -18.95583473709188382, 37.95507249208304756 ) ) ;
#15799 = LINE ( 'NONE', #2552, #3122 ) ;
#15800 = CARTESIAN_POINT ( 'NONE',  ( -17.68048971390462754, -22.64274437364856496, 31.61132249208304401 ) ) ;
#15801 = DIRECTION ( 'NONE',  ( 1.000000000000000000, -0.000000000000000000, 0.000000000000000000 ) ) ;
#15802 = VERTEX_POINT ( 'NONE', #533 ) ;
#15803 = PLANE ( 'NONE',  #4691 ) ;
#15804 = ORIENTED_EDGE ( 'NONE', *, *, #616, .T. ) ;
#15805 = LINE ( 'NONE', #5233, #16270 ) ;
#15806 = CARTESIAN_POINT ( 'NONE',  ( -14.99999999999999645, 47.00000000000000711, 23.99999999999997868 ) ) ;
#15807 = LINE ( 'NONE', #8543, #32 ) ;
#15808 = AXIS2_PLACEMENT_3D ( 'NONE', #8197, #5250, #6712 ) ;
#15809 = DIRECTION ( 'NONE',  ( -0.000000000000000000, -0.7071067811865456854, -0.7071067811865493491 ) ) ;
#15810 = CARTESIAN_POINT ( 'NONE',  ( -15.00000000000000000, 49.99999999999997158, -4.956352788505161414E-14 ) ) ;
#15811 = CARTESIAN_POINT ( 'NONE',  ( -9.098294960646575315E-15, 29.83102903476757817, 56.65425233947097894 ) ) ;
#15812 = FACE_OUTER_BOUND ( 'NONE', #4494, .T. ) ;
#15813 = VERTEX_POINT ( 'NONE', #8272 ) ;
#15814 = ORIENTED_EDGE ( 'NONE', *, *, #6424, .F. ) ;
#15815 = STYLED_ITEM ( 'NONE', ( #2888 ), #6657 ) ;
#15816 = CARTESIAN_POINT ( 'NONE',  ( -12.35725562635143682, -19.75228648362908501, 36.20117750791695954 ) ) ;
#15817 = AXIS2_PLACEMENT_3D ( 'NONE', #2915, #4594, #17818 ) ;
#15818 = CARTESIAN_POINT ( 'NONE',  ( -0.8561741729129465073, 61.93301270000000613, 48.10000000109246798 ) ) ;
#15819 = CARTESIAN_POINT ( 'NONE',  ( -12.35725562635140307, -28.24771351637085459, 29.42382249208304401 ) ) ;
#15820 = CARTESIAN_POINT ( 'NONE',  ( -8.528048594804062077, -45.28611686177728046, 3.000000000000000000 ) ) ;
#15821 = CARTESIAN_POINT ( 'NONE',  ( -19.24771351637089367, -21.35725562635142438, 34.88867750791696665 ) ) ;
#15822 = DIRECTION ( 'NONE',  ( -1.000000000000000000, 0.000000000000000000, -0.000000000000000000 ) ) ;
#15823 = CARTESIAN_POINT ( 'NONE',  ( -13.49542703274178201, -19.04416526290806289, 35.98242750791695954 ) ) ;
#15824 = FACE_OUTER_BOUND ( 'NONE', #16105, .T. ) ;
#15825 = CARTESIAN_POINT ( 'NONE',  ( -20.04416526290809131, -22.82508104294700502, 26.14257249208304046 ) ) ;
#15826 = CARTESIAN_POINT ( 'NONE',  ( 1.461580736456473906, 62.53841926354353120, 46.05000000109246372 ) ) ;
#15827 = CARTESIAN_POINT ( 'NONE',  ( -2.500000000000001776, 64.00000000000000000, 49.19999999999999574 ) ) ;
#15828 = EDGE_CURVE ( 'NONE', #5969, #10544, #3759, .T. ) ;
#15829 = CIRCLE ( 'NONE', #3931, 10.00000000000000178 ) ;
#15830 = VECTOR ( 'NONE', #9090, 1000.000000000000000 ) ;
#15831 = PRODUCT_DEFINITION_SHAPE ( 'NONE', 'NONE',  #19406 ) ;
#15832 = DIRECTION ( 'NONE',  ( -0.000000000000000000, -1.000000000000000000, -0.000000000000000000 ) ) ;
#15833 = CARTESIAN_POINT ( 'NONE',  ( -1.035533905932738641, 66.50000000000000000, 49.85000000000000142 ) ) ;
#15834 = CARTESIAN_POINT ( 'NONE',  ( -25.00000000000000000, 110.0000000000000000, -5.000000000000004441 ) ) ;
#15835 = ORIENTED_EDGE ( 'NONE', *, *, #17550, .T. ) ;
#15836 = EDGE_CURVE ( 'NONE', #16414, #16562, #18385, .T. ) ;
#15837 =( LENGTH_UNIT ( ) NAMED_UNIT ( * ) SI_UNIT ( .MILLI., .METRE. ) );
#15838 = CARTESIAN_POINT ( 'NONE',  ( 1.461580736456473684, 65.46158073645646880, 46.05000000109246372 ) ) ;
#15839 = CARTESIAN_POINT ( 'NONE',  ( -15.16482700510260706, -26.99999999999998579, 38.38867750791695954 ) ) ;
#15840 = CARTESIAN_POINT ( 'NONE',  ( -7.999999999999986677, 60.00000000000000711, 45.00000000000000000 ) ) ;
#15841 = CARTESIAN_POINT ( 'NONE',  ( -21.14459132904239169, -20.64274437364858628, 31.61132249208303691 ) ) ;
#15842 = AXIS2_PLACEMENT_3D ( 'NONE', #8979, #7021, #7118 ) ;
#15843 = VECTOR ( 'NONE', #2190, 1000.000000000000000 ) ;
#15844 = CARTESIAN_POINT ( 'NONE',  ( 2.066987300000001415, 64.00000000000000000, 48.55000000109247082 ) ) ;
#15845 = ORIENTED_EDGE ( 'NONE', *, *, #14999, .T. ) ;
#15846 = DIRECTION ( 'NONE',  ( 1.000000000000000000, 0.000000000000000000, 0.000000000000000000 ) ) ;
#15847 = DIRECTION ( 'NONE',  ( 1.000000000000000000, -0.000000000000000000, -0.000000000000000000 ) ) ;
#15848 = CARTESIAN_POINT ( 'NONE',  ( 1.461580736456473684, 65.46158073645646880, 47.65000000109247225 ) ) ;
#15849 = CARTESIAN_POINT ( 'NONE',  ( -50.00000000000002132, 3.000000000000000000, -60.00000000000002132 ) ) ;
#15850 = CARTESIAN_POINT ( 'NONE',  ( -1.040834085586084257E-14, 25.49999999999998934, 52.50000000000000000 ) ) ;
#15851 = ADVANCED_FACE ( 'NONE', ( #11291 ), #14332, .F. ) ;
#15852 = EDGE_CURVE ( 'NONE', #16168, #9690, #9816, .T. ) ;
#15853 = CARTESIAN_POINT ( 'NONE',  ( 5.199999999999996625, 3.306546357697854226E-16, 2.700000000000000622 ) ) ;
#15854 = EDGE_CURVE ( 'NONE', #15466, #11383, #17010, .T. ) ;
#15855 = VECTOR ( 'NONE', #4242, 1000.000000000000000 ) ;
#15856 = AXIS2_PLACEMENT_3D ( 'NONE', #11170, #8156, #17263 ) ;
#15857 = PLANE ( 'NONE',  #8333 ) ;
#15858 = ORIENTED_EDGE ( 'NONE', *, *, #18595, .T. ) ;
#15859 = VERTEX_POINT ( 'NONE', #11380 ) ;
#15860 = CARTESIAN_POINT ( 'NONE',  ( -15.16482700510258574, -30.99999999999998224, 38.38867750791694533 ) ) ;
#15861 = ORIENTED_EDGE ( 'NONE', *, *, #6743, .T. ) ;
#15863 = ORIENTED_EDGE ( 'NONE', *, *, #15261, .F. ) ;
#15862 = ORIENTED_EDGE ( 'NONE', *, *, #17741, .T. ) ;
#15864 = CARTESIAN_POINT ( 'NONE',  ( -17.68048971390462754, -22.64274437364856496, 42.11132249208304756 ) ) ;
#15865 = CARTESIAN_POINT ( 'NONE',  ( -11.64274437364854187, -30.14459132904234195, 27.45117750791696309 ) ) ;
#15866 = DIRECTION ( 'NONE',  ( 0.000000000000000000, 0.4999999999999992228, -0.8660254037844390407 ) ) ;
#15867 = CARTESIAN_POINT ( 'NONE',  ( -1.035533905932738863, 61.50000000000000000, 48.65000000218493881 ) ) ;
#15868 = CARTESIAN_POINT ( 'NONE',  ( 1.000000000000001332, -36.00000000000000711, 9.500000000000001776 ) ) ;
#15869 = VERTEX_POINT ( 'NONE', #17372 ) ;
#15870 = MECHANICAL_DESIGN_GEOMETRIC_PRESENTATION_REPRESENTATION (  '', ( #12096 ), #7739 ) ;
#15871 = DIRECTION ( 'NONE',  ( -6.672013369141567928E-17, 0.000000000000000000, 1.000000000000000000 ) ) ;
#15872 = ORIENTED_EDGE ( 'NONE', *, *, #10533, .T. ) ;
#15873 = DIRECTION ( 'NONE',  ( 1.000000000000000000, 0.000000000000000000, 0.000000000000000000 ) ) ;
#15874 = ORIENTED_EDGE ( 'NONE', *, *, #8436, .F. ) ;
#15875 = CARTESIAN_POINT ( 'NONE',  ( -40.00000000000000711, 113.0000000000000000, 8.000000000000000000 ) ) ;
#15876 = LINE ( 'NONE', #4111, #7171 ) ;
#15877 = FACE_OUTER_BOUND ( 'NONE', #15609, .T. ) ;
#15878 = CARTESIAN_POINT ( 'NONE',  ( -2.066987300000001415, 63.14382582708705627, 44.80000000109247082 ) ) ;
#15879 = EDGE_CURVE ( 'NONE', #19310, #9095, #6483, .T. ) ;
#15880 = DIRECTION ( 'NONE',  ( 0.000000000000000000, -1.000000000000000000, 0.000000000000000000 ) ) ;
#15881 = LINE ( 'NONE', #2442, #17394 ) ;
#15882 = DIRECTION ( 'NONE',  ( 0.000000000000000000, 1.632680918566406793E-16, -1.000000000000000000 ) ) ;
#15883 = EDGE_LOOP ( 'NONE', ( #7644, #7173, #6789, #5000 ) ) ;
#15884 = ORIENTED_EDGE ( 'NONE', *, *, #15414, .T. ) ;
#15885 = CARTESIAN_POINT ( 'NONE',  ( -21.99999999999999289, -23.83517299489739116, 8.201177507916955989 ) ) ;
#15886 = DIRECTION ( 'NONE',  ( -0.000000000000000000, 1.000000000000000000, -0.000000000000000000 ) ) ;
#15887 = VERTEX_POINT ( 'NONE', #19141 ) ;
#15888 = CARTESIAN_POINT ( 'NONE',  ( -18.53959229564982536, -27.78091578003890660, 30.51757249208304401 ) ) ;
#15889 = CARTESIAN_POINT ( 'NONE',  ( -44.99999999999998579, 3.000000000000000000, -56.50000000000000000 ) ) ;
#15890 = ORIENTED_EDGE ( 'NONE', *, *, #3136, .T. ) ;
#15891 = CARTESIAN_POINT ( 'NONE',  ( -14.83517299489736985, -26.99999999999998579, 29.86132249208304756 ) ) ;
#15892 = CARTESIAN_POINT ( 'NONE',  ( -1.035533905932738641, 66.50000000000000000, 49.04999999999999716 ) ) ;
#15893 = EDGE_LOOP ( 'NONE', ( #10209, #18087, #17716, #13171 ) ) ;
#15894 = CARTESIAN_POINT ( 'NONE',  ( 5.799999999999985612, 29.65425233947092920, 56.47747564417436195 ) ) ;
#15895 = VERTEX_POINT ( 'NONE', #17463 ) ;
#15896 = EDGE_CURVE ( 'NONE', #3035, #13613, #828, .T. ) ;
#15897 = DIRECTION ( 'NONE',  ( 1.156482317317871725E-16, 0.000000000000000000, -1.000000000000000000 ) ) ;
#15898 = PLANE ( 'NONE',  #2654 ) ;
#15899 = LINE ( 'NONE', #2463, #12561 ) ;
#15900 = CARTESIAN_POINT ( 'NONE',  ( -12.35725562635143682, -19.75228648362908501, 30.95117750791695954 ) ) ;
#15901 = FACE_OUTER_BOUND ( 'NONE', #19322, .T. ) ;
#15902 = EDGE_CURVE ( 'NONE', #12841, #6570, #1189, .T. ) ;
#15903 = CARTESIAN_POINT ( 'NONE',  ( 49.99999999999998579, 0.000000000000000000, 59.99999999999997868 ) ) ;
#15904 = CARTESIAN_POINT ( 'NONE',  ( -14.83517299489739649, -18.99999999999997868, 9.513677507916957765 ) ) ;
#15905 = CARTESIAN_POINT ( 'NONE',  ( 24.99999999999998579, -6.000000000000000000, 42.49999999999997868 ) ) ;
#15906 = EDGE_LOOP ( 'NONE', ( #11057, #12950, #17340, #7528, #16962 ) ) ;
#15907 = UNCERTAINTY_MEASURE_WITH_UNIT (LENGTH_MEASURE( 1.000000000000000082E-05 ), #14288, 'distance_accuracy_value', 'NONE');
#15908 = SHAPE_REPRESENTATION ( 'Heating Element & carriage', ( #1791 ), #2707 ) ;
#15909 = CARTESIAN_POINT ( 'NONE',  ( -13.49542703274178379, -19.04416526290806289, 30.73242750791695599 ) ) ;
#15910 = CARTESIAN_POINT ( 'NONE',  ( 1.461580736456473684, 65.46158073645646880, 47.65000000109247225 ) ) ;
#15911 = CARTESIAN_POINT ( 'NONE',  ( -19.99999999999999645, -24.16482700510261949, 36.42382249208304046 ) ) ;
#15912 = VECTOR ( 'NONE', #4183, 1000.000000000000000 ) ;
#15913 = CARTESIAN_POINT ( 'NONE',  ( -2.066987300000001415, 63.14382582708705627, 44.80000000109247082 ) ) ;
#15914 = FACE_BOUND ( 'NONE', #12957, .T. ) ;
#15915 = EDGE_CURVE ( 'NONE', #16834, #10481, #8731, .T. ) ;
#15916 = CARTESIAN_POINT ( 'NONE',  ( -10.75228648362910100, -26.64274437364854009, 27.01367750791695954 ) ) ;
#15917 = LINE ( 'NONE', #13650, #3285 ) ;
#15918 = CARTESIAN_POINT ( 'NONE',  ( -13.82508104294698015, -29.04416526290806289, 27.66992750791695599 ) ) ;
#15919 = CARTESIAN_POINT ( 'NONE',  ( -32.50000000000000000, 53.00000000000000711, -32.35000000000001563 ) ) ;
#15920 = DIRECTION ( 'NONE',  ( -0.000000000000000000, -0.000000000000000000, -1.000000000000000000 ) ) ;
#15921 = VECTOR ( 'NONE', #16525, 1000.000000000000000 ) ;
#15922 = CARTESIAN_POINT ( 'NONE',  ( -2.066987300000001859, 64.85617417291294373, 44.90000000109247225 ) ) ;
#15923 = CARTESIAN_POINT ( 'NONE',  ( 0.8561741729129460632, 66.06698730000000808, 48.70000000109247651 ) ) ;
#15924 = DIRECTION ( 'NONE',  ( 0.000000000000000000, 0.000000000000000000, -1.000000000000000000 ) ) ;
#15925 = CARTESIAN_POINT ( 'NONE',  ( -2.500000000000001776, 65.03553390593273775, 49.95000000000000284 ) ) ;
#15926 = DIRECTION ( 'NONE',  ( 2.602085213965211135E-16, -1.000000000000000000, 0.000000000000000000 ) ) ;
#15927 = AXIS2_PLACEMENT_3D ( 'NONE', #6630, #12305, #6529 ) ;
#15928 = ORIENTED_EDGE ( 'NONE', *, *, #867, .T. ) ;
#15929 = CARTESIAN_POINT ( 'NONE',  ( 2.066987300000001859, 63.14382582708704916, 45.90000000109247225 ) ) ;
#15930 = CARTESIAN_POINT ( 'NONE',  ( -19.41254052147348830, -26.35725562635142083, 2.513677507916958209 ) ) ;
#15931 = CARTESIAN_POINT ( 'NONE',  ( 1.767766952966369987, 65.76776695296638309, 48.89999999999999858 ) ) ;
#15932 = CARTESIAN_POINT ( 'NONE',  ( -21.95583473709189803, -26.04047135212049469, 30.95507249208304401 ) ) ;
#15933 = VECTOR ( 'NONE', #19276, 1000.000000000000000 ) ;
#15934 = CARTESIAN_POINT ( 'NONE',  ( -2.066987300000001415, 64.00000000000000000, 44.75000000109247367 ) ) ;
#15935 = VERTEX_POINT ( 'NONE', #4337 ) ;
#15936 = DIRECTION ( 'NONE',  ( 3.493455720571401687E-15, 0.7071067811865496822, -0.7071067811865454633 ) ) ;
#15937 = DIRECTION ( 'NONE',  ( 0.000000000000000000, -1.000000000000000000, 0.000000000000000000 ) ) ;
#15938 = VECTOR ( 'NONE', #17164, 1000.000000000000000 ) ;
#15939 = CARTESIAN_POINT ( 'NONE',  ( 2.066987300000001859, 63.14382582708704916, 47.50000000109246656 ) ) ;
#15940 = CARTESIAN_POINT ( 'NONE',  ( 46.99999999999997868, 30.87867965644035806, 42.87867965644034740 ) ) ;
#15941 = ADVANCED_FACE ( 'NONE', ( #11672 ), #518, .T. ) ;
#15942 = EDGE_CURVE ( 'NONE', #15290, #10386, #16669, .T. ) ;
#15943 = CARTESIAN_POINT ( 'NONE',  ( -1.530808498934192803E-16, 66.50000000000000000, 49.10000000218494165 ) ) ;
#15944 = CARTESIAN_POINT ( 'NONE',  ( -41.00000000000000711, 110.0000000000000000, -37.50000000000000711 ) ) ;
#15945 = EDGE_CURVE ( 'NONE', #5878, #17254, #18883, .T. ) ;
#15946 = VECTOR ( 'NONE', #1481, 1000.000000000000000 ) ;
#15947 = PLANE ( 'NONE',  #4261 ) ;
#15948 = ORIENTED_EDGE ( 'NONE', *, *, #5654, .T. ) ;
#15949 = EDGE_LOOP ( 'NONE', ( #4910, #4987, #5005, #14035 ) ) ;
#15950 = CARTESIAN_POINT ( 'NONE',  ( -15.16482700510264436, -16.99999999999997868, 6.236322492083039570 ) ) ;
#15951 = ADVANCED_FACE ( 'NONE', ( #10494 ), #13344, .T. ) ;
#15952 = VECTOR ( 'NONE', #7681, 1000.000000000000000 ) ;
#15953 = VERTEX_POINT ( 'NONE', #10787 ) ;
#15954 = AXIS2_PLACEMENT_3D ( 'NONE', #14368, #1232, #7212 ) ;
#15956 = ORIENTED_EDGE ( 'NONE', *, *, #11695, .T. ) ;
#15955 = ORIENTED_EDGE ( 'NONE', *, *, #7108, .F. ) ;
#15957 = CARTESIAN_POINT ( 'NONE',  ( -17.68048971390461688, -25.35725562635141372, 7.763677507916960430 ) ) ;
#15958 = CARTESIAN_POINT ( 'NONE',  ( -16.71081734191527346, -16.95583473709190159, 30.29492750791696665 ) ) ;
#15959 = VECTOR ( 'NONE', #5199, 1000.000000000000000 ) ;
#15960 = DIRECTION ( 'NONE',  ( 0.000000000000000000, -1.000000000000000000, 1.287488025362403787E-15 ) ) ;
#15961 = CARTESIAN_POINT ( 'NONE',  ( -2.500000000000001776, 64.00000000000000000, 47.70000000218494307 ) ) ;
#15962 = CARTESIAN_POINT ( 'NONE',  ( -24.00000000000000000, 53.00000000000000711, 30.00000000000000000 ) ) ;
#15963 = ORIENTED_EDGE ( 'NONE', *, *, #6133, .T. ) ;
#15964 = EDGE_CURVE ( 'NONE', #11032, #15578, #16787, .T. ) ;
#15965 = CARTESIAN_POINT ( 'NONE',  ( 0.000000000000000000, -1.178949249685214307, 2.042000000000002036 ) ) ;
#15966 = ORIENTED_EDGE ( 'NONE', *, *, #8174, .F. ) ;
#15967 = CARTESIAN_POINT ( 'NONE',  ( -41.00000000000000711, 110.0000000000000000, -44.00000000000000000 ) ) ;
#15968 = VECTOR ( 'NONE', #13159, 1000.000000000000000 ) ;
#15969 = ORIENTED_EDGE ( 'NONE', *, *, #6076, .F. ) ;
#15970 = CARTESIAN_POINT ( 'NONE',  ( -1.805156233539796151, 62.95673454514856360, 44.99999999999999289 ) ) ;
#15971 = FACE_OUTER_BOUND ( 'NONE', #11883, .T. ) ;
#15972 = DIRECTION ( 'NONE',  ( -0.000000000000000000, 0.000000000000000000, -1.000000000000000000 ) ) ;
#15973 = AXIS2_PLACEMENT_3D ( 'NONE', #13478, #5938, #7702 ) ;
#15974 = CARTESIAN_POINT ( 'NONE',  ( 2.066987300000001859, 64.85617417291294373, 46.80000000109246372 ) ) ;
#15975 = EDGE_CURVE ( 'NONE', #10054, #1553, #1392, .T. ) ;
#15976 = DIRECTION ( 'NONE',  ( 0.000000000000000000, -1.000000000000000000, 0.000000000000000000 ) ) ;
#15977 = CARTESIAN_POINT ( 'NONE',  ( -41.00000000000000711, 113.0000000000000000, -50.00000000000000000 ) ) ;
#15978 = AXIS2_PLACEMENT_3D ( 'NONE', #9527, #2090, #14039 ) ;
#15979 = CARTESIAN_POINT ( 'NONE',  ( 0.9731771629430463477, 62.14345849393435373, 44.99999999999997868 ) ) ;
#15980 = ORIENTED_EDGE ( 'NONE', *, *, #2062, .F. ) ;
#15982 = EDGE_LOOP ( 'NONE', ( #3763, #15966, #18310, #8790 ) ) ;
#15981 = ORIENTED_EDGE ( 'NONE', *, *, #6865, .F. ) ;
#15983 = CARTESIAN_POINT ( 'NONE',  ( -11.35725562635144925, -18.02023567606020293, 4.701177507916955989 ) ) ;
#15984 = LINE ( 'NONE', #3835, #9907 ) ;
#15985 = VECTOR ( 'NONE', #13285, 1000.000000000000000 ) ;
#15986 = ORIENTED_EDGE ( 'NONE', *, *, #12356, .F. ) ;
#15987 = CARTESIAN_POINT ( 'NONE',  ( -12.92450931948790149, -21.68318583509881137, 6.892572492083043123 ) ) ;
#15988 = VECTOR ( 'NONE', #3357, 1000.000000000000000 ) ;
#15989 = EDGE_CURVE ( 'NONE', #5479, #13749, #4439, .T. ) ;
#15990 = EDGE_CURVE ( 'NONE', #14781, #3001, #14028, .T. ) ;
#15991 = DIRECTION ( 'NONE',  ( 0.000000000000000000, 0.000000000000000000, -1.000000000000000000 ) ) ;
#15992 = ORIENTED_EDGE ( 'NONE', *, *, #7601, .T. ) ;
#15993 = CARTESIAN_POINT ( 'NONE',  ( -17.31681416490115311, -26.07549068051209318, 2.294927507916959986 ) ) ;
#15994 = VERTEX_POINT ( 'NONE', #18363 ) ;
#15995 = VECTOR ( 'NONE', #1679, 1000.000000000000000 ) ;
#15996 = CARTESIAN_POINT ( 'NONE',  ( -1.035533905932738641, 66.50000000000000000, 46.75000000218494733 ) ) ;
#15997 = VERTEX_POINT ( 'NONE', #18456 ) ;
#15998 = FACE_OUTER_BOUND ( 'NONE', #3224, .T. ) ;
#15999 = EDGE_CURVE ( 'NONE', #8744, #576, #1339, .T. ) ;
#16000 = DIRECTION ( 'NONE',  ( -1.000000000000000000, 0.000000000000000000, -9.251858538542970348E-17 ) ) ;
#16001 = CARTESIAN_POINT ( 'NONE',  ( 4.592425496802577917E-16, 61.50000000000000000, 47.90000000218494591 ) ) ;
#16002 = VECTOR ( 'NONE', #672, 1000.000000000000114 ) ;
#16003 = CARTESIAN_POINT ( 'NONE',  ( 24.99999999999999289, -6.000000000000000000, -42.49999999999999289 ) ) ;
#16004 = CIRCLE ( 'NONE', #7550, 2.999999999999999112 ) ;
#16005 = CARTESIAN_POINT ( 'NONE',  ( -14.83517299489739649, -18.99999999999997868, 25.26367750791695599 ) ) ;
#16006 = FACE_BOUND ( 'NONE', #17917, .T. ) ;
#16007 = CARTESIAN_POINT ( 'NONE',  ( -10.04416526290807710, -25.50457296725819489, 5.794927507916955989 ) ) ;
#16008 = CLOSED_SHELL ( 'NONE', ( #785, #8781, #10224, #16708, #6622, #5879, #14037, #1750, #18644, #19222, #16297, #14890, #17998, #16817, #13955, #9540, #7012, #14527, #12520, #2723, #3986, #17625, #2633, #11054, #15616, #12402, #19132, #1903, #10894, #14033, #8951, #10398, #6280, #12594, #18285, #14024, #17987, #2310, #5098, #17782, #12496, #7990, #13659, #4262, #6039, #5096, #378, #6907 ) ) ;
#16009 = DIRECTION ( 'NONE',  ( 0.000000000000000000, 0.000000000000000000, -1.000000000000000000 ) ) ;
#16010 = VERTEX_POINT ( 'NONE', #600 ) ;
#16011 = EDGE_CURVE ( 'NONE', #18238, #11126, #4921, .T. ) ;
#16012 = CARTESIAN_POINT ( 'NONE',  ( -19.99999999999999645, -24.16482700510261949, 4.923822492083040459 ) ) ;
#16013 = VECTOR ( 'NONE', #13676, 1000.000000000000000 ) ;
#16014 = CARTESIAN_POINT ( 'NONE',  ( -7.999999999999996447, -24.16482700510256976, 0.3261775079169564884 ) ) ;
#16015 = CARTESIAN_POINT ( 'NONE',  ( -2.066987300000001415, 64.00000000000000000, 47.95000000109246940 ) ) ;
#16016 = CARTESIAN_POINT ( 'NONE',  ( -12.35725562635140307, -28.24771351637085459, 34.67382249208304046 ) ) ;
#16017 = CARTESIAN_POINT ( 'NONE',  ( 0.000000000000000000, 0.000000000000000000, 0.000000000000000000 ) ) ;
#16018 = VERTEX_POINT ( 'NONE', #9323 ) ;
#16019 = DIRECTION ( 'NONE',  ( 4.898042755699219393E-16, -0.000000000000000000, 1.000000000000000000 ) ) ;
#16020 = CARTESIAN_POINT ( 'NONE',  ( -19.24771351637089367, -21.35725562635142438, 24.38867750791695954 ) ) ;
#16021 = PLANE ( 'NONE',  #17991 ) ;
#16022 = CARTESIAN_POINT ( 'NONE',  ( -14.83517299489739649, -18.99999999999997868, 41.01367750791696665 ) ) ;
#16023 = CYLINDRICAL_SURFACE ( 'NONE', #4032, 2.500000000000001776 ) ;
#16024 = CARTESIAN_POINT ( 'NONE',  ( -18.78091578003892792, -20.46040770435013556, 42.33007249208303335 ) ) ;
#16025 = CARTESIAN_POINT ( 'NONE',  ( 2.500000000000001776, 65.03553390593273775, 47.24999999999999289 ) ) ;
#16026 = DIRECTION ( 'NONE',  ( 0.000000000000000000, 1.000000000000000000, 0.000000000000000000 ) ) ;
#16027 = CYLINDRICAL_SURFACE ( 'NONE', #15247, 2.649999999999992806 ) ;
#16028 = CARTESIAN_POINT ( 'NONE',  ( 2.066987300000002303, 63.14382582708705627, 46.10000000109246798 ) ) ;
#16029 = CARTESIAN_POINT ( 'NONE',  ( -41.00000000000000711, 110.0000000000000000, -30.99999999999999645 ) ) ;
#16030 =( BOUNDED_CURVE ( )  B_SPLINE_CURVE ( 2, ( #9796, #6954, #18919, #11450, #19016, #7143, #19112, #4013, #5582 ),
 .UNSPECIFIED., .F., .F. ) 
 B_SPLINE_CURVE_WITH_KNOTS ( ( 3, 2, 2, 2, 3 ),
 ( 0.07142857142857121644, 0.08928571428571414892, 0.1071428571428570675, 0.1250000000000000000, 0.1428571428571429047 ),
 .UNSPECIFIED. ) 
 CURVE ( )  GEOMETRIC_REPRESENTATION_ITEM ( )  RATIONAL_B_SPLINE_CURVE ( ( 1.000000000000000666, 0.9238795325112857393, 1.000000000000000000, 0.9238795325112867385, 1.000000000000000000, 0.9238795325112867385, 1.000000000000000000, 0.9238795325112865164, 1.000000000000000222 ) ) 
 REPRESENTATION_ITEM ( '' )  );
#16031 = ADVANCED_FACE ( 'NONE', ( #9424 ), #12562, .T. ) ;
#16032 = ORIENTED_EDGE ( 'NONE', *, *, #6499, .F. ) ;
#16033 = CARTESIAN_POINT ( 'NONE',  ( 1.461580736456473906, 62.53841926354353120, 45.05000000109246372 ) ) ;
#16034 = CARTESIAN_POINT ( 'NONE',  ( -11.99999999999999289, -24.16482700510258752, 37.07617750791695954 ) ) ;
#16035 = PLANE ( 'NONE',  #1640 ) ;
#16036 = CARTESIAN_POINT ( 'NONE',  ( -13.28918265808478694, -16.95583473709189093, 27.45507249208304046 ) ) ;
#16037 = CARTESIAN_POINT ( 'NONE',  ( -2.066987300000001859, 64.85617417291294373, 49.70000000109248361 ) ) ;
#16038 = CARTESIAN_POINT ( 'NONE',  ( -14.03132541760401786, -21.04416526290806289, 25.48242750791696309 ) ) ;
#16039 = CARTESIAN_POINT ( 'NONE',  ( -11.46040770435012490, -27.78091578003888173, 6.232427507916957765 ) ) ;
#16040 = CARTESIAN_POINT ( 'NONE',  ( 14.99999999999998579, 3.000000000000000000, 20.99999999999997513 ) ) ;
#16041 = CARTESIAN_POINT ( 'NONE',  ( -1.461580736456473462, 62.53841926354353120, 45.65000000109247225 ) ) ;
#16042 = DIRECTION ( 'NONE',  ( -1.000000000000000000, -0.000000000000000000, -0.000000000000000000 ) ) ;
#16043 = DIRECTION ( 'NONE',  ( -0.000000000000000000, 1.000000000000000000, -0.000000000000000000 ) ) ;
#16044 = LINE ( 'NONE', #2604, #4421 ) ;
#16045 = CARTESIAN_POINT ( 'NONE',  ( 7.500000000000005329, -38.00000000000000000, 12.50000000000000000 ) ) ;
#16046 = VERTEX_POINT ( 'NONE', #10889 ) ;
#16047 = ORIENTED_EDGE ( 'NONE', *, *, #12486, .T. ) ;
#16048 = CARTESIAN_POINT ( 'NONE',  ( -18.64274437364860049, -18.02023567606023491, 5.798822492083038682 ) ) ;
#16049 = ORIENTED_EDGE ( 'NONE', *, *, #4371, .T. ) ;
#16051 = EDGE_LOOP ( 'NONE', ( #8367, #8406, #1473, #2643, #7745, #9799 ) ) ;
#16050 = EDGE_LOOP ( 'NONE', ( #10406, #3119, #12191, #7397, #17159 ) ) ;
#16052 = CARTESIAN_POINT ( 'NONE',  ( -17.51566270880201159, -22.35725562635141728, 3.388677507916959986 ) ) ;
#16053 = CARTESIAN_POINT ( 'NONE',  ( -11.35725562635144925, -18.02023567606020293, 36.20117750791695244 ) ) ;
#16054 = CARTESIAN_POINT ( 'NONE',  ( 41.99999999999997868, 139.6861997365471950, 51.99999999999997868 ) ) ;
#16055 = CARTESIAN_POINT ( 'NONE',  ( 1.461580736456473906, 62.53841926354353120, 48.25000000109246656 ) ) ;
#16056 = DIRECTION ( 'NONE',  ( -0.000000000000000000, -1.000000000000000000, -0.000000000000000000 ) ) ;
#16057 = ORIENTED_EDGE ( 'NONE', *, *, #11323, .F. ) ;
#16058 = CARTESIAN_POINT ( 'NONE',  ( -41.00000000000000711, 53.00000000000000711, 20.00000000000000000 ) ) ;
#16059 = ORIENTED_EDGE ( 'NONE', *, *, #8414, .F. ) ;
#16060 = CARTESIAN_POINT ( 'NONE',  ( -25.00000000000000000, 53.00000000000000711, 30.00000000000000000 ) ) ;
#16061 = VERTEX_POINT ( 'NONE', #14029 ) ;
#16062 = FACE_OUTER_BOUND ( 'NONE', #4907, .T. ) ;
#16063 = CARTESIAN_POINT ( 'NONE',  ( -40.00000000000000711, 53.00000000000000711, -18.00000000000000000 ) ) ;
#16064 = LINE ( 'NONE', #5679, #2472 ) ;
#16065 = ADVANCED_FACE ( 'NONE', ( #16884 ), #5302, .F. ) ;
#16066 = CARTESIAN_POINT ( 'NONE',  ( 1.461580736456473684, 65.46158073645646880, 45.25000000109247367 ) ) ;
#16067 = LINE ( 'NONE', #11735, #15667 ) ;
#16068 = CARTESIAN_POINT ( 'NONE',  ( -44.99999999999998579, -1.285879139104706187E-16, -55.00000000000000000 ) ) ;
#16069 = PLANE ( 'NONE',  #10163 ) ;
#16070 = EDGE_LOOP ( 'NONE', ( #3402, #14780, #12519, #7647 ) ) ;
#16072 = ORIENTED_EDGE ( 'NONE', *, *, #1361, .F. ) ;
#16071 = ORIENTED_EDGE ( 'NONE', *, *, #12084, .T. ) ;
#16073 = CARTESIAN_POINT ( 'NONE',  ( -15.16482700510258574, -30.99999999999998224, 1.638677507916956433 ) ) ;
#16074 = LINE ( 'NONE', #12836, #824 ) ;
#16075 = EDGE_LOOP ( 'NONE', ( #10739, #2240, #14480 ) ) ;
#16076 = CARTESIAN_POINT ( 'NONE',  ( -12.35725562635140307, -28.24771351637085459, 39.92382249208304046 ) ) ;
#16077 = EDGE_CURVE ( 'NONE', #18550, #13312, #1142, .T. ) ;
#16078 = LINE ( 'NONE', #14138, #3103 ) ;
#16079 = ORIENTED_EDGE ( 'NONE', *, *, #17798, .F. ) ;
#16080 = CARTESIAN_POINT ( 'NONE',  ( -14.36097942780923731, -27.04416526290806999, 6.669927507916960430 ) ) ;
#16081 = CARTESIAN_POINT ( 'NONE',  ( -50.00000000000001421, 3.000000000000000000, 59.99999999999997868 ) ) ;
#16082 = VERTEX_POINT ( 'NONE', #3641 ) ;
#16083 = DIRECTION ( 'NONE',  ( 0.000000000000000000, 0.000000000000000000, 1.000000000000000000 ) ) ;
#16084 = ORIENTED_EDGE ( 'NONE', *, *, #3524, .F. ) ;
#16085 = CARTESIAN_POINT ( 'NONE',  ( -40.00000000000000711, 113.0000000000000000, 13.49999999999999822 ) ) ;
#16086 = CARTESIAN_POINT ( 'NONE',  ( -41.00000000000000711, 53.00000000000000711, -12.50000000000000000 ) ) ;
#16087 = CARTESIAN_POINT ( 'NONE',  ( 1.300000000000000044, 1.478016689125442484, -1.626303258728256651E-15 ) ) ;
#16088 = FACE_OUTER_BOUND ( 'NONE', #13509, .T. ) ;
#16089 = EDGE_CURVE ( 'NONE', #14781, #9140, #13027, .T. ) ;
#16090 = CARTESIAN_POINT ( 'NONE',  ( -17.64274437364855430, -28.24771351637087236, 23.07617750791695954 ) ) ;
#16091 = EDGE_CURVE ( 'NONE', #8804, #17825, #9612, .T. ) ;
#16092 =( GEOMETRIC_REPRESENTATION_CONTEXT ( 3 ) GLOBAL_UNCERTAINTY_ASSIGNED_CONTEXT ( ( #9637 ) ) GLOBAL_UNIT_ASSIGNED_CONTEXT ( ( #16512, #4264, #13364 ) ) REPRESENTATION_CONTEXT ( 'NONE', 'WORKASPACE' ) );
#16093 = CARTESIAN_POINT ( 'NONE',  ( 0.000000000000000000, 0.000000000000000000, 0.000000000000000000 ) ) ;
#16094 = EDGE_CURVE ( 'NONE', #11949, #3590, #6592, .T. ) ;
#16095 = CARTESIAN_POINT ( 'NONE',  ( -10.04416526290807710, -25.50457296725819489, 0.5449275079169579872 ) ) ;
#16096 = DIRECTION ( 'NONE',  ( -1.000000000000000000, 0.000000000000000000, 0.000000000000000000 ) ) ;
#16097 = ORIENTED_EDGE ( 'NONE', *, *, #9414, .T. ) ;
#16098 = PRODUCT_DEFINITION_CONTEXT ( 'detailed design', #13704, 'design' ) ;
#16099 = CARTESIAN_POINT ( 'NONE',  ( -18.78091578003892081, -20.46040770435013556, 10.83007249208303691 ) ) ;
#16100 = CARTESIAN_POINT ( 'NONE',  ( -14.83517299489739649, -18.99999999999997868, 41.01367750791696665 ) ) ;
#16101 = CARTESIAN_POINT ( 'NONE',  ( -0.8561741729129461742, 66.06698729999999387, 47.00000000109247367 ) ) ;
#16102 = CARTESIAN_POINT ( 'NONE',  ( -15.63902057219073605, -27.04416526290807710, 3.830072492083042679 ) ) ;
#16103 = COLOUR_RGB ( '', 0.66274510, 0.83137255, 0.94901961) ;
#16104 = DIRECTION ( 'NONE',  ( 0.000000000000000000, 0.000000000000000000, 1.000000000000000000 ) ) ;
#16105 = EDGE_LOOP ( 'NONE', ( #4711, #2848, #4651, #4227 ) ) ;
#16106 = VECTOR ( 'NONE', #17301, 1000.000000000000000 ) ;
#16107 = CARTESIAN_POINT ( 'NONE',  ( 0.000000000000000000, 47.00000000000000711, -67.72004514666936359 ) ) ;
#16108 = LINE ( 'NONE', #13451, #16254 ) ;
#16109 = DIRECTION ( 'NONE',  ( -1.000000000000000000, 0.000000000000000000, 0.000000000000000000 ) ) ;
#16110 = CYLINDRICAL_SURFACE ( 'NONE', #7512, 2.649999999999992806 ) ;
#16111 = LINE ( 'NONE', #39, #599 ) ;
#16112 = CARTESIAN_POINT ( 'NONE',  ( -19.41254052147350961, -21.64274437364857562, 36.86132249208304046 ) ) ;
#16113 = ADVANCED_FACE ( 'NONE', ( #9704 ), #12363, .F. ) ;
#16114 = EDGE_CURVE ( 'NONE', #2938, #9711, #11460, .T. ) ;
#16115 = CARTESIAN_POINT ( 'NONE',  ( 1.035533905932738197, 66.50000000000000000, 47.34999999999999432 ) ) ;
#16116 = CARTESIAN_POINT ( 'NONE',  ( 1.461580736456473684, 65.46158073645646880, 49.45000000109246940 ) ) ;
#16117 = LINE ( 'NONE', #9835, #7986 ) ;
#16118 = CARTESIAN_POINT ( 'NONE',  ( -2.500000000000001776, 64.00000000000000000, 46.00000000000000000 ) ) ;
#16119 = CARTESIAN_POINT ( 'NONE',  ( 49.99999999999998579, 118.0000000000000142, 59.99999999999997868 ) ) ;
#16120 = AXIS2_PLACEMENT_3D ( 'NONE', #15806, #14329, #19134 ) ;
#16121 = ORIENTED_EDGE ( 'NONE', *, *, #14904, .T. ) ;
#16122 = CARTESIAN_POINT ( 'NONE',  ( -19.99999999999999645, -23.83517299489738051, 2.951177507916958209 ) ) ;
#16123 = CARTESIAN_POINT ( 'NONE',  ( -15.63902057219076269, -20.95583473709189448, 40.79492750791695244 ) ) ;
#16124 = CARTESIAN_POINT ( 'NONE',  ( -41.99999999999997868, 3.000000000000002665, 51.99999999999997868 ) ) ;
#16125 = CARTESIAN_POINT ( 'NONE',  ( -18.64274437364860049, -18.02023567606023491, 42.54882249208304046 ) ) ;
#16126 = CARTESIAN_POINT ( 'NONE',  ( 1.461580736456473684, 65.46158073645646880, 47.05000000109247082 ) ) ;
#16127 = CARTESIAN_POINT ( 'NONE',  ( -13.35725562635142794, -21.48433729119796709, 36.20117750791695954 ) ) ;
#16128 = VECTOR ( 'NONE', #7338, 1000.000000000000000 ) ;
#16129 = CARTESIAN_POINT ( 'NONE',  ( -11.46040770435012490, -27.78091578003888173, 0.9824275079169582092 ) ) ;
#16130 = CARTESIAN_POINT ( 'NONE',  ( -31.74999999999995737, 0.000000000000000000, 0.000000000000000000 ) ) ;
#16131 = VECTOR ( 'NONE', #15163, 1000.000000000000000 ) ;
#16132 = ADVANCED_FACE ( 'NONE', ( #3731 ), #2267, .T. ) ;
#16133 = CARTESIAN_POINT ( 'NONE',  ( 0.000000000000000000, -52.00000000000000711, 1.500000000000000000 ) ) ;
#16134 = CARTESIAN_POINT ( 'NONE',  ( 19.09188309203663891, 29.56586399182256741, 56.56586399182270952 ) ) ;
#16135 =( BOUNDED_CURVE ( )  B_SPLINE_CURVE ( 2, ( #373, #16543, #7526, #4693, #15082, #4398, #12025, #82, #6257 ),
 .UNSPECIFIED., .F., .F. ) 
 B_SPLINE_CURVE_WITH_KNOTS ( ( 3, 2, 2, 2, 3 ),
 ( 0.2857142857142853098, 0.3035714285714282701, 0.3214285714285712858, 0.3392857142857143016, 0.3571428571428572618 ),
 .UNSPECIFIED. ) 
 CURVE ( )  GEOMETRIC_REPRESENTATION_ITEM ( )  RATIONAL_B_SPLINE_CURVE ( ( 1.000000000000001554, 0.9238795325112850731, 1.000000000000000000, 0.9238795325112867385, 1.000000000000000000, 0.9238795325112867385, 1.000000000000000000, 0.9238795325112862944, 1.000000000000000444 ) ) 
 REPRESENTATION_ITEM ( '' )  );
#16136 = DIRECTION ( 'NONE',  ( 0.000000000000000000, 0.000000000000000000, 1.000000000000000000 ) ) ;
#16137 = CARTESIAN_POINT ( 'NONE',  ( 1.461580736456473684, 65.46158073645646880, 47.85000000109246798 ) ) ;
#16138 = DIRECTION ( 'NONE',  ( 0.000000000000000000, 0.000000000000000000, -1.000000000000000000 ) ) ;
#16139 = CARTESIAN_POINT ( 'NONE',  ( 3.399999999999996803, 29.65425233947092920, 56.47747564417434774 ) ) ;
#16140 = VERTEX_POINT ( 'NONE', #8252 ) ;
#16141 = ORIENTED_EDGE ( 'NONE', *, *, #1859, .F. ) ;
#16142 = CARTESIAN_POINT ( 'NONE',  ( -11.35725562635139418, -29.97976432393972601, 3.173822492083039126 ) ) ;
#16143 = VECTOR ( 'NONE', #12624, 1000.000000000000000 ) ;
#16144 = ORIENTED_EDGE ( 'NONE', *, *, #18974, .T. ) ;
#16145 = CIRCLE ( 'NONE', #2087, 2.999999999999999112 ) ;
#16146 = PLANE ( 'NONE',  #16933 ) ;
#16148 = ORIENTED_EDGE ( 'NONE', *, *, #17534, .T. ) ;
#16147 = ORIENTED_EDGE ( 'NONE', *, *, #16188, .F. ) ;
#16149 = CARTESIAN_POINT ( 'NONE',  ( -14.03132541760401786, -21.04416526290806289, -0.7675724920830402365 ) ) ;
#16150 = CARTESIAN_POINT ( 'NONE',  ( -15.16482700510258574, -30.99999999999998224, 38.38867750791694533 ) ) ;
#16151 = CARTESIAN_POINT ( 'NONE',  ( -2.750000000000020872, 118.0000000000000142, -42.68883962248118991 ) ) ;
#16152 = CARTESIAN_POINT ( 'NONE',  ( -1.767766952966370209, 65.76776695296638309, 45.20000000218494307 ) ) ;
#16153 = CARTESIAN_POINT ( 'NONE',  ( -47.00000000000001421, 16.75735931288065572, 56.99999999999997158 ) ) ;
#16154 = ORIENTED_EDGE ( 'NONE', *, *, #2439, .T. ) ;
#16155 = DIRECTION ( 'NONE',  ( 0.000000000000000000, 0.000000000000000000, 1.000000000000000000 ) ) ;
#16156 = ORIENTED_EDGE ( 'NONE', *, *, #12530, .F. ) ;
#16157 = ORIENTED_EDGE ( 'NONE', *, *, #10373, .F. ) ;
#16158 = CARTESIAN_POINT ( 'NONE',  ( -35.00000000000002132, -6.000000000000000000, -47.50000000000002132 ) ) ;
#16159 = PLANE ( 'NONE',  #18131 ) ;
#16160 = DIRECTION ( 'NONE',  ( -1.048036716171419796E-14, -0.7071067811865496822, 0.7071067811865454633 ) ) ;
#16161 = CIRCLE ( 'NONE', #12413, 2.649999999999985700 ) ;
#16162 = CARTESIAN_POINT ( 'NONE',  ( -2.066987300000001859, 64.85617417291294373, 44.70000000109248361 ) ) ;
#16163 = AXIS2_PLACEMENT_3D ( 'NONE', #13735, #118, #317 ) ;
#16164 = DIRECTION ( 'NONE',  ( -0.000000000000000000, 1.000000000000000000, -0.000000000000000000 ) ) ;
#16165 = PLANE ( 'NONE',  #2370 ) ;
#16166 = DIRECTION ( 'NONE',  ( -0.000000000000000000, -1.000000000000000000, -0.000000000000000000 ) ) ;
#16167 = EDGE_LOOP ( 'NONE', ( #7023, #4300, #2649, #8241, #11095, #8761, #16144, #15675, #12445, #13589, #2638, #15512, #494, #11941, #10666, #18076, #5723, #4006, #3367, #3465, #3820, #18365, #17488, #950, #5503, #7221, #7152, #17330, #2142, #10790, #15173, #8993, #3810, #15045, #17629, #12042, #1735, #3436, #16753, #2444, #13863, #16370, #9011, #9180, #15125, #14291, #8827, #5146, #5540, #1893, #18909, #14578 ) ) ;
#16169 = ORIENTED_EDGE ( 'NONE', *, *, #14048, .T. ) ;
#16168 = VERTEX_POINT ( 'NONE', #14221 ) ;
#16170 = CARTESIAN_POINT ( 'NONE',  ( -15.16482700510258574, -30.99999999999998224, 6.888677507916956877 ) ) ;
#16171 = DIRECTION ( 'NONE',  ( -0.000000000000000000, -1.000000000000000000, -0.000000000000000000 ) ) ;
#16172 = EDGE_LOOP ( 'NONE', ( #1246, #13908, #15007, #6058 ) ) ;
#16173 = ORIENTED_EDGE ( 'NONE', *, *, #11748, .F. ) ;
#16174 = CARTESIAN_POINT ( 'NONE',  ( -14.83517299489735741, -28.99999999999998224, 40.36132249208304046 ) ) ;
#16175 = AXIS2_PLACEMENT_3D ( 'NONE', #6566, #8043, #3234 ) ;
#16176 = CARTESIAN_POINT ( 'NONE',  ( 8.000000000000003553, -32.00000000000000711, 1.500000000000000000 ) ) ;
#16177 = ORIENTED_EDGE ( 'NONE', *, *, #4697, .F. ) ;
#16178 = CARTESIAN_POINT ( 'NONE',  ( -17.95583473709190869, -24.96867458239598037, 41.45507249208304046 ) ) ;
#16179 = CARTESIAN_POINT ( 'NONE',  ( -1.035533905932738641, 66.50000000000000000, 44.35000000218494165 ) ) ;
#16180 = ORIENTED_EDGE ( 'NONE', *, *, #13911, .T. ) ;
#16181 = PLANE ( 'NONE',  #14708 ) ;
#16182 = EDGE_LOOP ( 'NONE', ( #17614, #8683, #15986, #6158 ) ) ;
#16183 = CARTESIAN_POINT ( 'NONE',  ( 0.08838834764830674762, 29.80514068711925901, 56.68014068711929809 ) ) ;
#16184 = CARTESIAN_POINT ( 'NONE',  ( 2.500000000000001776, 64.00000000000000000, 49.99999999999999289 ) ) ;
#16185 = CARTESIAN_POINT ( 'NONE',  ( 1.300000000000000044, 0.000000000000000000, 0.000000000000000000 ) ) ;
#16186 = CARTESIAN_POINT ( 'NONE',  ( -15.00000000000000000, -35.50000000000000711, 8.000000000000007105 ) ) ;
#16187 = ADVANCED_FACE ( 'NONE', ( #789 ), #18560, .T. ) ;
#16188 = EDGE_CURVE ( 'NONE', #1873, #14646, #5128, .T. ) ;
#16189 = COLOUR_RGB ( '', 0.31764706, 0.68627451, 0.89019608) ;
#16190 = CARTESIAN_POINT ( 'NONE',  ( -11.21908421996108629, -20.46040770435011069, 31.16992750791695599 ) ) ;
#16191 = FACE_OUTER_BOUND ( 'NONE', #100, .T. ) ;
#16192 = CARTESIAN_POINT ( 'NONE',  ( -13.82508104294698192, -29.04416526290806644, 1.419927507916958209 ) ) ;
#16193 = CYLINDRICAL_SURFACE ( 'NONE', #5839, 2.500000000000001776 ) ;
#16194 = ORIENTED_EDGE ( 'NONE', *, *, #11793, .T. ) ;
#16195 = CARTESIAN_POINT ( 'NONE',  ( -11.35725562635139418, -29.97976432393972601, 39.92382249208304046 ) ) ;
#16196 = CARTESIAN_POINT ( 'NONE',  ( -12.95952864787955150, -17.04416526290805933, 9.732427507916955989 ) ) ;
#16197 = CARTESIAN_POINT ( 'NONE',  ( 0.8561741729129472844, 61.93301270000000613, 45.80000000109246372 ) ) ;
#16198 = CARTESIAN_POINT ( 'NONE',  ( -12.92450931948790149, -21.68318583509881137, 1.642572492083043123 ) ) ;
#16199 = CARTESIAN_POINT ( 'NONE',  ( -1.461580736456473462, 62.53841926354353120, 44.85000000109246798 ) ) ;
#16200 = VERTEX_POINT ( 'NONE', #6396 ) ;
#16201 = EDGE_CURVE ( 'NONE', #17270, #5689, #13930, .T. ) ;
#16202 = LINE ( 'NONE', #14735, #15952 ) ;
#16203 = PLANE ( 'NONE',  #7185 ) ;
#16204 = ADVANCED_FACE ( 'NONE', ( #13633 ), #9224, .T. ) ;
#16205 = DIRECTION ( 'NONE',  ( 0.000000000000000000, 1.000000000000000000, 0.000000000000000000 ) ) ;
#16206 = CARTESIAN_POINT ( 'NONE',  ( 1.300000000000000044, -0.7390083445627200209, 1.280000000000001137 ) ) ;
#16207 = LINE ( 'NONE', #13360, #5602 ) ;
#16208 = CARTESIAN_POINT ( 'NONE',  ( -9.999999999999994671, -23.83517299489734143, 39.04882249208304046 ) ) ;
#16209 = CARTESIAN_POINT ( 'NONE',  ( -2.500000000000000888, 62.96446609406726935, 46.04999999999999005 ) ) ;
#16210 = CARTESIAN_POINT ( 'NONE',  ( -2.066987300000001415, 64.85617417291294373, 47.30000000109247082 ) ) ;
#16211 = FACE_OUTER_BOUND ( 'NONE', #6569, .T. ) ;
#16212 = CARTESIAN_POINT ( 'NONE',  ( -1.035533905932738641, 66.50000000000000000, 47.44999999999999574 ) ) ;
#16213 = DIRECTION ( 'NONE',  ( -1.000000000000000000, -0.000000000000000000, -0.000000000000000000 ) ) ;
#16214 = ORIENTED_EDGE ( 'NONE', *, *, #2551, .F. ) ;
#16215 = FACE_OUTER_BOUND ( 'NONE', #4541, .T. ) ;
#16216 = CARTESIAN_POINT ( 'NONE',  ( -15.16482700510259640, -28.99999999999998224, 1.638677507916958431 ) ) ;
#16217 = CARTESIAN_POINT ( 'NONE',  ( -2.067357986984026397, 63.55004841362024592, 44.99999999999997868 ) ) ;
#16218 = CARTESIAN_POINT ( 'NONE',  ( -18.53959229564982536, -27.78091578003890660, 9.517572492083042235 ) ) ;
#16219 = EDGE_CURVE ( 'NONE', #10251, #9405, #3151, .T. ) ;
#16220 = ADVANCED_FACE ( 'NONE', ( #18359 ), #3252, .T. ) ;
#16221 = CARTESIAN_POINT ( 'NONE',  ( -1.461580736456473906, 65.46158073645646880, 44.65000000109246514 ) ) ;
#16222 = CARTESIAN_POINT ( 'NONE',  ( -12.64274437364855252, -28.41254052147347053, 1.201177507916958431 ) ) ;
#16223 = CARTESIAN_POINT ( 'NONE',  ( -18.53959229564986799, -20.21908421996107563, 3.607427507916957321 ) ) ;
#16224 = CARTESIAN_POINT ( 'NONE',  ( -4.012830983233618198, 32.52836399182267257, 53.60336399182263989 ) ) ;
#16225 = EDGE_CURVE ( 'NONE', #6936, #6193, #15307, .T. ) ;
#16226 = CARTESIAN_POINT ( 'NONE',  ( 14.99999999999998579, 73.00000000000001421, 26.99999999999997158 ) ) ;
#16227 = CARTESIAN_POINT ( 'NONE',  ( 8.000000000000014211, 60.00000000000000711, 45.00000000000000000 ) ) ;
#16228 = VECTOR ( 'NONE', #8393, 1000.000000000000000 ) ;
#16229 = DIRECTION ( 'NONE',  ( -1.000000000000000000, -0.000000000000000000, -0.000000000000000000 ) ) ;
#16230 = CARTESIAN_POINT ( 'NONE',  ( -0.8561741729129466183, 61.93301270000000613, 48.30000000109247082 ) ) ;
#16231 = CARTESIAN_POINT ( 'NONE',  ( 4.012354697599942455, 32.70432772728315740, 53.78000129688596331 ) ) ;
#16232 = CARTESIAN_POINT ( 'NONE',  ( 46.99999999999998579, 30.00000000000000355, 43.75735931288070191 ) ) ;
#16233 = ORIENTED_EDGE ( 'NONE', *, *, #14542, .F. ) ;
#16234 = ORIENTED_EDGE ( 'NONE', *, *, #16680, .T. ) ;
#16235 = CARTESIAN_POINT ( 'NONE',  ( -20.97976432393974022, -27.64274437364858628, 14.98632249208303868 ) ) ;
#16236 = VECTOR ( 'NONE', #11732, 1000.000000000000227 ) ;
#16237 = PLANE ( 'NONE',  #3469 ) ;
#16239 = ORIENTED_EDGE ( 'NONE', *, *, #14751, .T. ) ;
#16238 = ORIENTED_EDGE ( 'NONE', *, *, #259, .T. ) ;
#16240 = EDGE_CURVE ( 'NONE', #5462, #6482, #3026, .T. ) ;
#16241 = CARTESIAN_POINT ( 'NONE',  ( -15.16482700510260706, -26.99999999999998579, 1.638677507916960208 ) ) ;
#16242 = CARTESIAN_POINT ( 'NONE',  ( -20.97976432393974022, -27.64274437364858628, 4.486322492083039570 ) ) ;
#16243 = VECTOR ( 'NONE', #14166, 1000.000000000000000 ) ;
#16244 = DIRECTION ( 'NONE',  ( 0.000000000000000000, -0.000000000000000000, 1.000000000000000000 ) ) ;
#16245 = CARTESIAN_POINT ( 'NONE',  ( -0.8561741729129461742, 66.06698729999999387, 48.60000000109246798 ) ) ;
#16246 = ORIENTED_EDGE ( 'NONE', *, *, #821, .F. ) ;
#16247 = VERTEX_POINT ( 'NONE', #1981 ) ;
#16248 = CARTESIAN_POINT ( 'NONE',  ( 4.592425496802577917E-16, 61.50000000000000000, 46.19999999999999574 ) ) ;
#16249 = LINE ( 'NONE', #18649, #18529 ) ;
#16250 = ORIENTED_EDGE ( 'NONE', *, *, #7567, .T. ) ;
#16251 = CARTESIAN_POINT ( 'NONE',  ( -15.00000000000000000, -37.50000000000000000, 7.499999999999995559 ) ) ;
#16252 = DIRECTION ( 'NONE',  ( -7.709882115452476934E-17, -0.000000000000000000, -1.000000000000000000 ) ) ;
#16253 = PLANE ( 'NONE',  #9975 ) ;
#16254 = VECTOR ( 'NONE', #1202, 1000.000000000000000 ) ;
#16255 = CARTESIAN_POINT ( 'NONE',  ( -2.066987300000001415, 63.14382582708705627, 48.20000000109247651 ) ) ;
#16256 = PRODUCT_DEFINITION ( 'UNKNOWN', '', #11413, #8843 ) ;
#16257 = DIRECTION ( 'NONE',  ( 0.000000000000000000, 0.000000000000000000, 1.000000000000000000 ) ) ;
#16258 = CIRCLE ( 'NONE', #15639, 1.500000000000000222 ) ;
#16259 = VECTOR ( 'NONE', #5093, 1000.000000000000000 ) ;
#16260 = DIRECTION ( 'NONE',  ( 0.000000000000000000, 1.000000000000000000, 0.000000000000000000 ) ) ;
#16261 = EDGE_LOOP ( 'NONE', ( #2244, #2531 ) ) ;
#16263 = ORIENTED_EDGE ( 'NONE', *, *, #12876, .T. ) ;
#16262 = VERTEX_POINT ( 'NONE', #218 ) ;
#16264 = CARTESIAN_POINT ( 'NONE',  ( -19.95583473709191580, -22.49542703274176603, 39.91992750791695954 ) ) ;
#16265 = LINE ( 'NONE', #13222, #7413 ) ;
#16266 = ORIENTED_EDGE ( 'NONE', *, *, #16407, .T. ) ;
#16267 = VECTOR ( 'NONE', #12052, 1000.000000000000000 ) ;
#16268 = ORIENTED_EDGE ( 'NONE', *, *, #5203, .T. ) ;
#16269 = CARTESIAN_POINT ( 'NONE',  ( -11.95583473709190514, -24.63902057219072361, 2.517572492083043123 ) ) ;
#16270 = VECTOR ( 'NONE', #15897, 1000.000000000000000 ) ;
#16271 = CARTESIAN_POINT ( 'NONE',  ( 44.99999999999997158, 6.000000000000000000, 56.50000000000000000 ) ) ;
#16272 = FACE_OUTER_BOUND ( 'NONE', #1699, .T. ) ;
#16273 = ORIENTED_EDGE ( 'NONE', *, *, #8794, .F. ) ;
#16274 = CARTESIAN_POINT ( 'NONE',  ( -16.35725562635142794, -21.31951028609535470, 3.826177507916959986 ) ) ;
#16275 = VECTOR ( 'NONE', #17253, 1000.000000000000000 ) ;
#16276 = CARTESIAN_POINT ( 'NONE',  ( 50.00000000000000000, 118.0000000000000142, -60.00000000000000000 ) ) ;
#16277 = ORIENTED_EDGE ( 'NONE', *, *, #3988, .T. ) ;
#16278 = DIRECTION ( 'NONE',  ( 1.000000000000000000, -0.000000000000000000, 0.000000000000000000 ) ) ;
#16279 = VERTEX_POINT ( 'NONE', #4832 ) ;
#16280 = DIRECTION ( 'NONE',  ( -0.000000000000000000, -1.000000000000000000, -0.000000000000000000 ) ) ;
#16281 = CARTESIAN_POINT ( 'NONE',  ( -4.744034285469996171, -45.28611686177728046, 3.000000000000000000 ) ) ;
#16282 = CARTESIAN_POINT ( 'NONE',  ( 32.50000000000000000, -6.000000000000000000, -45.00000000000000000 ) ) ;
#16283 = VECTOR ( 'NONE', #11092, 1000.000000000000000 ) ;
#16284 = DIRECTION ( 'NONE',  ( 1.000000000000000000, -0.000000000000000000, -0.000000000000000000 ) ) ;
#16285 = CARTESIAN_POINT ( 'NONE',  ( -12.35725562635143682, -19.75228648362908501, 25.70117750791695599 ) ) ;
#16286 = DIRECTION ( 'NONE',  ( -1.000000000000000000, 0.000000000000000000, 0.000000000000000000 ) ) ;
#16287 = CARTESIAN_POINT ( 'NONE',  ( -12.35725562635143682, -19.75228648362908501, 4.701177507916957765 ) ) ;
#16288 = VECTOR ( 'NONE', #6397, 1000.000000000000000 ) ;
#16289 = PLANE ( 'NONE',  #7077 ) ;
#16290 = ORIENTED_EDGE ( 'NONE', *, *, #7625, .T. ) ;
#16291 = UNCERTAINTY_MEASURE_WITH_UNIT (LENGTH_MEASURE( 1.000000000000000082E-05 ), #11213, 'distance_accuracy_value', 'NONE');
#16292 = CARTESIAN_POINT ( 'NONE',  ( -18.53959229564982536, -27.78091578003890660, 4.267572492083038682 ) ) ;
#16293 = CARTESIAN_POINT ( 'NONE',  ( -16.71081734191527346, -16.95583473709190159, 4.044927507916956877 ) ) ;
#16294 = CIRCLE ( 'NONE', #9731, 1.000000000000000000 ) ;
#16295 = CARTESIAN_POINT ( 'NONE',  ( 2.066987300000001859, 64.85617417291294373, 45.20000000109248361 ) ) ;
#16296 = ADVANCED_FACE ( 'NONE', ( #1885 ), #411, .F. ) ;
#16297 = ADVANCED_FACE ( 'NONE', ( #12360 ), #10782, .F. ) ;
#16298 = CARTESIAN_POINT ( 'NONE',  ( -13.35725562635141195, -26.51566270880198672, 3.173822492083044011 ) ) ;
#16299 = DIRECTION ( 'NONE',  ( 0.000000000000000000, 0.000000000000000000, -1.000000000000000000 ) ) ;
#16300 = ORIENTED_EDGE ( 'NONE', *, *, #1702, .F. ) ;
#16301 = VECTOR ( 'NONE', #13651, 1000.000000000000000 ) ;
#16302 = CARTESIAN_POINT ( 'NONE',  ( -11.42876933740184775, -19.36634849019432991, 1.100789300500590883E-12 ) ) ;
#16303 = ORIENTED_EDGE ( 'NONE', *, *, #14649, .T. ) ;
#16304 = CARTESIAN_POINT ( 'NONE',  ( -0.9999999999999945599, -36.00000000000000711, 9.500000000000001776 ) ) ;
#16305 = EDGE_CURVE ( 'NONE', #2520, #18340, #315, .T. ) ;
#16306 = CARTESIAN_POINT ( 'NONE',  ( 1.300000000000000044, -0.7390083445627200209, 1.280000000000001137 ) ) ;
#16307 = CARTESIAN_POINT ( 'NONE',  ( -2.500000000000001776, 64.00000000000000000, 45.30000000218493739 ) ) ;
#16308 = AXIS2_PLACEMENT_3D ( 'NONE', #15281, #2706, #5555 ) ;
#16309 = DIRECTION ( 'NONE',  ( -0.000000000000000000, 0.000000000000000000, -1.000000000000000000 ) ) ;
#16310 = CARTESIAN_POINT ( 'NONE',  ( -18.78091578003892792, -20.46040770435013556, 37.08007249208304046 ) ) ;
#16311 = CARTESIAN_POINT ( 'NONE',  ( -2.500000000000001776, 64.00000000000000000, 46.00000000000000000 ) ) ;
#16312 = CARTESIAN_POINT ( 'NONE',  ( -0.8561741729129461742, 66.06698730000000808, 46.40000000109247225 ) ) ;
#16313 = EDGE_CURVE ( 'NONE', #5670, #3722, #3356, .T. ) ;
#16314 = VECTOR ( 'NONE', #13507, 1000.000000000000000 ) ;
#16315 = PRODUCT ( 'Lever Press Handle Knob', 'Lever Press Handle Knob', '', ( #19137 ) ) ;
#16316 = DIRECTION ( 'NONE',  ( -0.000000000000000000, 1.000000000000000000, -0.000000000000000000 ) ) ;
#16317 = CARTESIAN_POINT ( 'NONE',  ( 1.035533905932739751, 61.50000000000000000, 47.04999999999999005 ) ) ;
#16318 = CARTESIAN_POINT ( 'NONE',  ( -5.800000000000006928, 29.65425233947099315, 56.47747564417430510 ) ) ;
#16319 = VECTOR ( 'NONE', #7985, 1000.000000000000000 ) ;
#16320 = ORIENTED_EDGE ( 'NONE', *, *, #14262, .T. ) ;
#16321 = VECTOR ( 'NONE', #16875, 1000.000000000000000 ) ;
#16322 = DIRECTION ( 'NONE',  ( 1.000000000000000000, 0.000000000000000000, 0.000000000000000000 ) ) ;
#16323 = CARTESIAN_POINT ( 'NONE',  ( -17.64274437364855430, -28.24771351637087236, 7.326177507916957765 ) ) ;
#16324 = CARTESIAN_POINT ( 'NONE',  ( -18.78091578003889950, -27.53959229564985378, 18.04492750791695954 ) ) ;
#16325 = CARTESIAN_POINT ( 'NONE',  ( -1.035533905932738641, 66.50000000000000000, 47.55000000218494449 ) ) ;
#16326 = CARTESIAN_POINT ( 'NONE',  ( -20.97976432393974022, -27.64274437364858628, 41.23632249208304046 ) ) ;
#16327 = VECTOR ( 'NONE', #380, 1000.000000000000000 ) ;
#16328 = CARTESIAN_POINT ( 'NONE',  ( 0.08332044287237951041, 33.84354269072930776, 52.64046917798810910 ) ) ;
#16329 = CARTESIAN_POINT ( 'NONE',  ( -19.41254052147348830, -26.35725562635142083, 2.513677507916958209 ) ) ;
#16330 = CARTESIAN_POINT ( 'NONE',  ( -10.75228648362910100, -26.64274437364854009, 11.26367750791695777 ) ) ;
#16331 = CARTESIAN_POINT ( 'NONE',  ( -43.50000000000000000, 118.0000000000000142, 32.50000000000000000 ) ) ;
#16332 = AXIS2_PLACEMENT_3D ( 'NONE', #10242, #8974, #2800 ) ;
#16333 = LINE ( 'NONE', #13482, #13108 ) ;
#16334 = DIRECTION ( 'NONE',  ( -0.000000000000000000, -0.000000000000000000, 1.000000000000000000 ) ) ;
#16335 = AXIS2_PLACEMENT_3D ( 'NONE', #11902, #1425, #10423 ) ;
#16336 = DIRECTION ( 'NONE',  ( -0.000000000000000000, 0.000000000000000000, 1.000000000000000000 ) ) ;
#16337 = DIRECTION ( 'NONE',  ( 0.000000000000000000, -0.4999999999999993894, 0.8660254037844389297 ) ) ;
#16338 = DIRECTION ( 'NONE',  ( -1.000000000000000000, -0.000000000000000000, -0.000000000000000000 ) ) ;
#16339 = EDGE_CURVE ( 'NONE', #19196, #3058, #4531, .T. ) ;
#16340 = ADVANCED_FACE ( 'NONE', ( #3448 ), #12456, .T. ) ;
#16341 = CARTESIAN_POINT ( 'NONE',  ( -9.183694056713489507E-15, 20.55025253169413091, 61.69238815542511389 ) ) ;
#16342 = EDGE_LOOP ( 'NONE', ( #19315, #19391, #17708, #17738 ) ) ;
#16343 = ORIENTED_EDGE ( 'NONE', *, *, #1109, .T. ) ;
#16344 = EDGE_CURVE ( 'NONE', #3100, #6543, #2076, .T. ) ;
#16345 = CARTESIAN_POINT ( 'NONE',  ( -11.64274437364859693, -17.85540867095757989, 22.42382249208304046 ) ) ;
#16346 = CARTESIAN_POINT ( 'NONE',  ( -24.00000000000000711, 53.00000000000000711, 8.000000000000000000 ) ) ;
#16348 = ORIENTED_EDGE ( 'NONE', *, *, #10430, .T. ) ;
#16347 = EDGE_LOOP ( 'NONE', ( #5834, #4513, #7657, #4938 ) ) ;
#16349 = CARTESIAN_POINT ( 'NONE',  ( -12.31951028609537602, -22.64274437364854364, 20.88867750791696309 ) ) ;
#16350 = DIRECTION ( 'NONE',  ( 0.000000000000000000, -0.000000000000000000, -1.000000000000000000 ) ) ;
#16351 = CARTESIAN_POINT ( 'NONE',  ( -17.04047135212050890, -17.04416526290807710, 6.017572492083039570 ) ) ;
#16352 = AXIS2_PLACEMENT_3D ( 'NONE', #16447, #2917, #1551 ) ;
#16353 = LINE ( 'NONE', #7826, #5385 ) ;
#16354 = CARTESIAN_POINT ( 'NONE',  ( -2.066987300000001415, 63.14382582708705627, 48.80000000109247082 ) ) ;
#16355 = ORIENTED_EDGE ( 'NONE', *, *, #12708, .T. ) ;
#16356 = VERTEX_POINT ( 'NONE', #18160 ) ;
#16357 = DIRECTION ( 'NONE',  ( 1.000000000000000000, -0.000000000000000000, -0.000000000000000000 ) ) ;
#16358 = DIRECTION ( 'NONE',  ( -1.000000000000000000, 0.000000000000000000, 0.000000000000000000 ) ) ;
#16359 = VECTOR ( 'NONE', #11138, 1000.000000000000000 ) ;
#16360 = ORIENTED_EDGE ( 'NONE', *, *, #3628, .F. ) ;
#16361 = FACE_OUTER_BOUND ( 'NONE', #3426, .T. ) ;
#16362 = LINE ( 'NONE', #9000, #14379 ) ;
#16363 = CARTESIAN_POINT ( 'NONE',  ( 1.461580736456473684, 65.46158073645646880, 47.85000000109246798 ) ) ;
#16364 = EDGE_CURVE ( 'NONE', #301, #8629, #4735, .T. ) ;
#16365 = EDGE_CURVE ( 'NONE', #17276, #3630, #19294, .T. ) ;
#16366 = DIRECTION ( 'NONE',  ( 0.000000000000000000, 0.000000000000000000, 1.000000000000000000 ) ) ;
#16367 = CARTESIAN_POINT ( 'NONE',  ( -32.50000000000000000, 53.00000000000000711, -37.64999999999999147 ) ) ;
#16368 = VERTEX_POINT ( 'NONE', #4384 ) ;
#16370 = ORIENTED_EDGE ( 'NONE', *, *, #8898, .T. ) ;
#16369 = VERTEX_POINT ( 'NONE', #7411 ) ;
#16371 = CARTESIAN_POINT ( 'NONE',  ( -8.855408670957631401, -20.64274437364852943, 10.38867750791695599 ) ) ;
#16372 = DIRECTION ( 'NONE',  ( -0.000000000000000000, -0.000000000000000000, -1.000000000000000000 ) ) ;
#16373 = ORIENTED_EDGE ( 'NONE', *, *, #14519, .F. ) ;
#16374 = ORIENTED_EDGE ( 'NONE', *, *, #3571, .T. ) ;
#16375 = CARTESIAN_POINT ( 'NONE',  ( -13.64274437364857739, -21.31951028609534760, 22.42382249208304401 ) ) ;
#16376 =( BOUNDED_CURVE ( )  B_SPLINE_CURVE ( 2, ( #405, #6197, #6290, #4825, #4728, #10774, #16682, #3245, #6388 ),
 .UNSPECIFIED., .F., .F. ) 
 B_SPLINE_CURVE_WITH_KNOTS ( ( 3, 2, 2, 2, 3 ),
 ( 0.7857142857142856984, 0.8035714285714286031, 0.8214285714285713969, 0.8392857142857141906, 0.8571428571428569843 ),
 .UNSPECIFIED. ) 
 CURVE ( )  GEOMETRIC_REPRESENTATION_ITEM ( )  RATIONAL_B_SPLINE_CURVE ( ( 1.000000000000000000, 0.9238795325112867385, 1.000000000000000000, 0.9238795325112867385, 1.000000000000000000, 0.9238795325112867385, 1.000000000000000000, 0.9238795325112871826, 0.9999999999999995559 ) ) 
 REPRESENTATION_ITEM ( '' )  );
#16377 = CYLINDRICAL_SURFACE ( 'NONE', #11230, 2.999999999999999112 ) ;
#16378 = CARTESIAN_POINT ( 'NONE',  ( -50.00000000000002132, 3.000000000000000000, -60.00000000000002132 ) ) ;
#16379 = EDGE_LOOP ( 'NONE', ( #865, #1472, #6911, #6583 ) ) ;
#16380 = CARTESIAN_POINT ( 'NONE',  ( -14.36097942780923731, -27.04416526290806999, 1.419927507916959986 ) ) ;
#16381 = CARTESIAN_POINT ( 'NONE',  ( -1.530808498934192803E-16, 66.50000000000000000, 44.30000000218494449 ) ) ;
#16382 = VERTEX_POINT ( 'NONE', #5849 ) ;
#16383 = CARTESIAN_POINT ( 'NONE',  ( -41.00000000000000711, 53.00000000000000711, -11.50000000000000000 ) ) ;
#16384 = VERTEX_POINT ( 'NONE', #14962 ) ;
#16385 = FACE_OUTER_BOUND ( 'NONE', #16749, .T. ) ;
#16386 = FACE_OUTER_BOUND ( 'NONE', #2630, .T. ) ;
#16387 = CYLINDRICAL_SURFACE ( 'NONE', #4755, 2.500000000000001776 ) ;
#16388 = EDGE_CURVE ( 'NONE', #3397, #9204, #210, .T. ) ;
#16389 = APPLICATION_PROTOCOL_DEFINITION ( 'draft international standard', 'automotive_design', 1998, #10703 ) ;
#16390 = CARTESIAN_POINT ( 'NONE',  ( 4.592425496802577917E-16, 61.50000000000000000, 46.30000000218493739 ) ) ;
#16391 = CARTESIAN_POINT ( 'NONE',  ( -4.012354697599992193, 26.78000129688593134, 59.70432772728315740 ) ) ;
#16392 = CARTESIAN_POINT ( 'NONE',  ( -25.00000000000000000, 53.00000000000000711, 30.00000000000000000 ) ) ;
#16393 = CARTESIAN_POINT ( 'NONE',  ( -12.35725562635143682, -19.75228648362908501, 15.20117750791695777 ) ) ;
#16394 = DIRECTION ( 'NONE',  ( 0.000000000000000000, -1.000000000000000000, 0.000000000000000000 ) ) ;
#16395 = ORIENTED_EDGE ( 'NONE', *, *, #18595, .F. ) ;
#16396 = CARTESIAN_POINT ( 'NONE',  ( -9.999999999999994671, -23.83517299489734143, 7.548822492083041347 ) ) ;
#16397 = CARTESIAN_POINT ( 'NONE',  ( -1.035533905932738863, 61.50000000000000000, 47.85000000218494165 ) ) ;
#16398 = CARTESIAN_POINT ( 'NONE',  ( -15.63902057219073605, -27.04416526290807710, 9.080072492083042235 ) ) ;
#16399 = FACE_OUTER_BOUND ( 'NONE', #13697, .T. ) ;
#16400 = ORIENTED_EDGE ( 'NONE', *, *, #1400, .F. ) ;
#16401 = CARTESIAN_POINT ( 'NONE',  ( -10.24659852207731170, -22.21293927426971493, 2.322403871605816317E-12 ) ) ;
#16402 = ORIENTED_EDGE ( 'NONE', *, *, #16802, .T. ) ;
#16403 = FACE_OUTER_BOUND ( 'NONE', #11334, .T. ) ;
#16404 = DIRECTION ( 'NONE',  ( -1.000000000000000000, -0.000000000000000000, -0.000000000000000000 ) ) ;
#16405 = CARTESIAN_POINT ( 'NONE',  ( -1.530808498934192803E-16, 66.50000000000000000, 45.10000000218494165 ) ) ;
#16406 = FACE_BOUND ( 'NONE', #4845, .T. ) ;
#16407 = EDGE_CURVE ( 'NONE', #8108, #6956, #12107, .T. ) ;
#16408 = CARTESIAN_POINT ( 'NONE',  ( -24.00000000000000711, 110.0000000000000000, -30.99999999999999645 ) ) ;
#16409 = EDGE_CURVE ( 'NONE', #10157, #14775, #4677, .T. ) ;
#16410 = CARTESIAN_POINT ( 'NONE',  ( 0.8561741729129460632, 66.06698730000000808, 46.30000000109247082 ) ) ;
#16411 = FACE_OUTER_BOUND ( 'NONE', #1241, .T. ) ;
#16412 = CARTESIAN_POINT ( 'NONE',  ( 2.500000000000002220, 62.96446609406726935, 47.94999999999999574 ) ) ;
#16413 = DIRECTION ( 'NONE',  ( -1.000000000000000000, 0.000000000000000000, 0.000000000000000000 ) ) ;
#16414 = VERTEX_POINT ( 'NONE', #16431 ) ;
#16415 = SURFACE_SIDE_STYLE ('',( #17596 ) ) ;
#16416 = CARTESIAN_POINT ( 'NONE',  ( -14.83517299489739649, -18.99999999999997868, 9.513677507916957765 ) ) ;
#16417 = CARTESIAN_POINT ( 'NONE',  ( -13.82508104294698192, -29.04416526290806644, 17.16992750791694888 ) ) ;
#16418 = CARTESIAN_POINT ( 'NONE',  ( -2.152366392613727974, 63.91624855416898043, 44.99999999999999289 ) ) ;
#16419 = CARTESIAN_POINT ( 'NONE',  ( -9.999999999999994671, -23.83517299489734143, 2.298822492083040903 ) ) ;
#16420 = CARTESIAN_POINT ( 'NONE',  ( 3.796994071234847710E-16, 61.93301269999999903, 46.75000000109246656 ) ) ;
#16421 = CARTESIAN_POINT ( 'NONE',  ( -17.51566270880201159, -22.35725562635141728, 40.13867750791696665 ) ) ;
#16422 = ADVANCED_FACE ( 'NONE', ( #16637 ), #6242, .T. ) ;
#16423 = CARTESIAN_POINT ( 'NONE',  ( 7.500000000000005329, -26.00000000000000000, 9.500000000000001776 ) ) ;
#16424 = CARTESIAN_POINT ( 'NONE',  ( -19.41254052147348830, -26.35725562635142083, 2.513677507916958209 ) ) ;
#16425 = PLANE ( 'NONE',  #3410 ) ;
#16426 = CARTESIAN_POINT ( 'NONE',  ( 0.8561741729129460632, 66.06698729999999387, 49.50000000109246656 ) ) ;
#16427 = DIRECTION ( 'NONE',  ( 0.000000000000000000, 0.000000000000000000, 1.000000000000000000 ) ) ;
#16428 = CARTESIAN_POINT ( 'NONE',  ( -7.499999999999994671, -26.00000000000000355, 4.500000000000000888 ) ) ;
#16429 = DIRECTION ( 'NONE',  ( 1.000000000000000000, 0.000000000000000000, 0.000000000000000000 ) ) ;
#16430 = AXIS2_PLACEMENT_3D ( 'NONE', #16706, #6025, #19350 ) ;
#16431 = CARTESIAN_POINT ( 'NONE',  ( 3.099999999999998757, 1.836970198721030181E-16, -1.500000000000000222 ) ) ;
#16432 = CARTESIAN_POINT ( 'NONE',  ( -32.50000000000002132, 0.000000000000000000, 24.99999999999998224 ) ) ;
#16433 = ADVANCED_FACE ( 'NONE', ( #8877 ), #2696, .T. ) ;
#16434 = CARTESIAN_POINT ( 'NONE',  ( -41.00000000000000711, 110.0000000000000000, 8.000000000000000000 ) ) ;
#16435 = ORIENTED_EDGE ( 'NONE', *, *, #16365, .F. ) ;
#16436 = ORIENTED_EDGE ( 'NONE', *, *, #6683, .F. ) ;
#16437 = CARTESIAN_POINT ( 'NONE',  ( -20.00369391078757886, -29.24501739517668142, 20.01757249208303691 ) ) ;
#16438 = SURFACE_STYLE_FILL_AREA ( #10053 ) ;
#16439 = LINE ( 'NONE', #13387, #15985 ) ;
#16441 = VERTEX_POINT ( 'NONE', #12208 ) ;
#16440 = EDGE_LOOP ( 'NONE', ( #1740, #10839, #2863, #9410 ) ) ;
#16442 = CARTESIAN_POINT ( 'NONE',  ( -13.64274437364856141, -26.68048971390460622, 11.70117750791696132 ) ) ;
#16443 = LINE ( 'NONE', #18019, #11738 ) ;
#16444 = CARTESIAN_POINT ( 'NONE',  ( -17.04047135212043784, -30.95583473709190159, 38.60742750791695954 ) ) ;
#16445 = VECTOR ( 'NONE', #2831, 1000.000000000000000 ) ;
#16446 = AXIS2_PLACEMENT_3D ( 'NONE', #17860, #4732, #4530 ) ;
#16447 = CARTESIAN_POINT ( 'NONE',  ( -45.00000000000000000, 3.000000000000000000, 54.99999999999998579 ) ) ;
#16448 = CARTESIAN_POINT ( 'NONE',  ( -1.767766952966369765, 62.23223304703363112, 44.60000000218494165 ) ) ;
#16449 = VERTEX_POINT ( 'NONE', #18209 ) ;
#16450 = ORIENTED_EDGE ( 'NONE', *, *, #14389, .T. ) ;
#16451 = CARTESIAN_POINT ( 'NONE',  ( -2.499999999999996003, 62.96446609406726225, 46.04999999999999005 ) ) ;
#16452 = CARTESIAN_POINT ( 'NONE',  ( -25.00000000000000711, 110.0000000000000000, -12.50000000000000000 ) ) ;
#16453 = EDGE_CURVE ( 'NONE', #3017, #6733, #13278, .T. ) ;
#16454 = ORIENTED_EDGE ( 'NONE', *, *, #1919, .F. ) ;
#16455 = CARTESIAN_POINT ( 'NONE',  ( -10.31147837279037738, -22.25502639194775512, -4.119453415160654225E-17 ) ) ;
#16456 = LINE ( 'NONE', #4703, #12500 ) ;
#16457 = ADVANCED_FACE ( 'NONE', ( #19375 ), #7808, .T. ) ;
#16458 = CARTESIAN_POINT ( 'NONE',  ( 3.796994071234847710E-16, 61.93301269999999903, 49.15000000109246514 ) ) ;
#16459 =( REPRESENTATION_RELATIONSHIP ('NONE','NONE', #7912, #6533 ) REPRESENTATION_RELATIONSHIP_WITH_TRANSFORMATION ( #3545 )SHAPE_REPRESENTATION_RELATIONSHIP( ) );
#16460 = CARTESIAN_POINT ( 'NONE',  ( -25.00000000000000711, 53.00000000000000711, -19.00000000000000000 ) ) ;
#16461 = VECTOR ( 'NONE', #3055, 1000.000000000000000 ) ;
#16462 = VECTOR ( 'NONE', #3313, 1000.000000000000000 ) ;
#16463 = DIRECTION ( 'NONE',  ( 0.000000000000000000, 0.000000000000000000, -1.000000000000000000 ) ) ;
#16464 = ORIENTED_EDGE ( 'NONE', *, *, #5549, .T. ) ;
#16466 = VERTEX_POINT ( 'NONE', #15452 ) ;
#16465 = ORIENTED_EDGE ( 'NONE', *, *, #11988, .F. ) ;
#16467 = CARTESIAN_POINT ( 'NONE',  ( -11.35725562635144925, -18.02023567606020293, 15.20117750791695599 ) ) ;
#16468 = CARTESIAN_POINT ( 'NONE',  ( 46.99999999999998579, 118.0000000000000142, 59.99999999999997868 ) ) ;
#16469 = ORIENTED_EDGE ( 'NONE', *, *, #15381, .T. ) ;
#16470 = ORIENTED_EDGE ( 'NONE', *, *, #18839, .F. ) ;
#16471 = CARTESIAN_POINT ( 'NONE',  ( -15.96867458239599635, -21.04416526290806999, 11.26757249208304579 ) ) ;
#16472 = LINE ( 'NONE', #9015, #18768 ) ;
#16473 = CARTESIAN_POINT ( 'NONE',  ( -2.499999999999996003, 62.96446609406726225, 46.95000000218494307 ) ) ;
#16474 = EDGE_LOOP ( 'NONE', ( #6352, #8842, #11136, #1650 ) ) ;
#16475 = CARTESIAN_POINT ( 'NONE',  ( -17.31681416490115311, -26.07549068051209318, 23.29492750791696309 ) ) ;
#16476 = AXIS2_PLACEMENT_3D ( 'NONE', #15622, #12481, #15069 ) ;
#16477 = CARTESIAN_POINT ( 'NONE',  ( 2.500000000000000000, -1.178949249685214307, 2.042000000000002036 ) ) ;
#16478 = ORIENTED_EDGE ( 'NONE', *, *, #14818, .T. ) ;
#16479 = ADVANCED_BREP_SHAPE_REPRESENTATION ( '', ( #3611, #1791 ), #9226 ) ;
#16480 = EDGE_CURVE ( 'NONE', #15286, #1273, #11123, .T. ) ;
#16481 = VECTOR ( 'NONE', #12503, 1000.000000000000000 ) ;
#16482 = DIRECTION ( 'NONE',  ( -1.000000000000000000, 0.000000000000000000, -0.000000000000000000 ) ) ;
#16483 = PRODUCT_DEFINITION_SHAPE ( 'NONE', 'NONE',  #19404 ) ;
#16484 = ORIENTED_EDGE ( 'NONE', *, *, #8356, .T. ) ;
#16485 = LINE ( 'NONE', #16085, #17245 ) ;
#16486 = LINE ( 'NONE', #2752, #18339 ) ;
#16487 = CARTESIAN_POINT ( 'NONE',  ( -24.00000000000000000, 53.00000000000000711, -5.000000000000004441 ) ) ;
#16488 = APPLICATION_PROTOCOL_DEFINITION ( 'draft international standard', 'automotive_design', 1998, #7058 ) ;
#16489 = CARTESIAN_POINT ( 'NONE',  ( 2.500000000000004441, 62.96446609406726225, 46.45000000218494307 ) ) ;
#16490 = CARTESIAN_POINT ( 'NONE',  ( -13.49542703274178379, -19.04416526290806289, 35.98242750791696665 ) ) ;
#16491 = DIRECTION ( 'NONE',  ( 0.000000000000000000, 1.000000000000000000, 0.000000000000000000 ) ) ;
#16492 = CARTESIAN_POINT ( 'NONE',  ( -17.64274437364855430, -28.24771351637087236, 23.07617750791695954 ) ) ;
#16493 = VECTOR ( 'NONE', #5132, 1000.000000000000000 ) ;
#16494 = CARTESIAN_POINT ( 'NONE',  ( 20.00000000000000355, -52.00000000000000711, 1.500000000000000000 ) ) ;
#16495 = VERTEX_POINT ( 'NONE', #6535 ) ;
#16496 = VECTOR ( 'NONE', #15116, 999.9999999999997726 ) ;
#16497 = UNCERTAINTY_MEASURE_WITH_UNIT (LENGTH_MEASURE( 1.000000000000000082E-05 ), #13368, 'distance_accuracy_value', 'NONE');
#16498 = CARTESIAN_POINT ( 'NONE',  ( -10.58745947852648328, -26.35725562635138530, 23.73632249208304046 ) ) ;
#16499 = EDGE_CURVE ( 'NONE', #16061, #10386, #646, .T. ) ;
#16500 = CARTESIAN_POINT ( 'NONE',  ( -1.265664690411616068E-16, 66.06698730000000808, 45.35000000109246798 ) ) ;
#16501 = CARTESIAN_POINT ( 'NONE',  ( -17.68048971390462754, -22.64274437364856496, 10.61132249208304401 ) ) ;
#16502 = LINE ( 'NONE', #19247, #10321 ) ;
#16503 = ORIENTED_EDGE ( 'NONE', *, *, #17741, .F. ) ;
#16504 = CARTESIAN_POINT ( 'NONE',  ( -10.14701344837433616, -21.92759952878850527, -1.842058582387526229E-17 ) ) ;
#16505 = ORIENTED_EDGE ( 'NONE', *, *, #11494, .T. ) ;
#16506 = CARTESIAN_POINT ( 'NONE',  ( -19.95583473709191580, -22.49542703274176603, 39.91992750791695954 ) ) ;
#16507 = CARTESIAN_POINT ( 'NONE',  ( 41.00000000000000000, 47.00000000000000711, 30.00000000000000000 ) ) ;
#16508 = FACE_OUTER_BOUND ( 'NONE', #11428, .T. ) ;
#16509 = DIRECTION ( 'NONE',  ( 0.000000000000000000, 0.000000000000000000, 1.000000000000000000 ) ) ;
#16510 = EDGE_CURVE ( 'NONE', #11826, #8366, #17119, .T. ) ;
#16511 = CARTESIAN_POINT ( 'NONE',  ( -2.066987300000000971, 63.14382582708704916, 48.20000000109247651 ) ) ;
#16512 =( LENGTH_UNIT ( ) NAMED_UNIT ( * ) SI_UNIT ( .MILLI., .METRE. ) );
#16513 = CARTESIAN_POINT ( 'NONE',  ( 1.767766952966370653, 62.23223304703363112, 45.50000000000000000 ) ) ;
#16514 = PLANE ( 'NONE',  #6143 ) ;
#16515 = EDGE_LOOP ( 'NONE', ( #3922, #17880, #1668, #19021 ) ) ;
#16516 = DIRECTION ( 'NONE',  ( 6.123233995736766036E-17, 1.000000000000000000, 0.000000000000000000 ) ) ;
#16517 = CARTESIAN_POINT ( 'NONE',  ( -12.35725562635143682, -19.75228648362908501, -0.5488224920830419018 ) ) ;
#16518 = CARTESIAN_POINT ( 'NONE',  ( -18.53959229564986799, -20.21908421996107563, 8.857427507916957765 ) ) ;
#16519 = CARTESIAN_POINT ( 'NONE',  ( 2.500000000000001776, 64.00000000000000000, 48.10000000218494165 ) ) ;
#16520 = CARTESIAN_POINT ( 'NONE',  ( -19.99999999999999645, -24.16482700510261949, 10.17382249208304046 ) ) ;
#16521 = CARTESIAN_POINT ( 'NONE',  ( -2.066987300000001415, 63.14382582708705627, 45.80000000109246372 ) ) ;
#16522 = CARTESIAN_POINT ( 'NONE',  ( -18.53959229564986799, -20.21908421996107563, 3.607427507916956877 ) ) ;
#16523 = DIRECTION ( 'NONE',  ( -0.000000000000000000, -1.000000000000000000, -0.000000000000000000 ) ) ;
#16524 = CARTESIAN_POINT ( 'NONE',  ( -18.78091578003889595, -27.53959229564985023, 18.04492750791695599 ) ) ;
#16525 = DIRECTION ( 'NONE',  ( -7.709882115452476934E-17, -0.000000000000000000, -1.000000000000000000 ) ) ;
#16526 = CARTESIAN_POINT ( 'NONE',  ( 32.50000000000000000, 47.00000000000000711, 15.00000000000000000 ) ) ;
#16527 = DIRECTION ( 'NONE',  ( -1.156482317317871478E-16, 1.000000000000000000, 0.000000000000000000 ) ) ;
#16528 = CARTESIAN_POINT ( 'NONE',  ( -25.00000000000000000, 53.00000000000000711, -31.00000000000000000 ) ) ;
#16529 = CARTESIAN_POINT ( 'NONE',  ( -1.909647267044692676, 63.20899822134837365, 45.00000000000000000 ) ) ;
#16530 = DIRECTION ( 'NONE',  ( -0.000000000000000000, -0.000000000000000000, -1.000000000000000000 ) ) ;
#16531 = DIRECTION ( 'NONE',  ( 0.000000000000000000, 0.000000000000000000, 1.000000000000000000 ) ) ;
#16532 = CARTESIAN_POINT ( 'NONE',  ( -41.00000000000000711, 53.00000000000000711, -24.49999999999999645 ) ) ;
#16533 = ORIENTED_EDGE ( 'NONE', *, *, #11767, .T. ) ;
#16534 = VERTEX_POINT ( 'NONE', #5160 ) ;
#16535 = CARTESIAN_POINT ( 'NONE',  ( -16.71081734191520596, -31.04416526290808065, 24.83007249208304046 ) ) ;
#16536 = MANIFOLD_SOLID_BREP ( 'Boss-Extrude3', #6349 ) ;
#16537 = CARTESIAN_POINT ( 'NONE',  ( -10.75228648362912232, -21.35725562635138530, 1.861322492083040903 ) ) ;
#16539 = VERTEX_POINT ( 'NONE', #11026 ) ;
#16538 = VERTEX_POINT ( 'NONE', #15642 ) ;
#16540 = CARTESIAN_POINT ( 'NONE',  ( -14.36097942780923731, -27.04416526290806999, 11.91992750791695954 ) ) ;
#16541 = PLANE ( 'NONE',  #17700 ) ;
#16542 = CARTESIAN_POINT ( 'NONE',  ( -15.16482700510264436, -16.99999999999997868, 6.236322492083039570 ) ) ;
#16543 = CARTESIAN_POINT ( 'NONE',  ( -2.500000000000019096, 65.03553390593272354, 48.35000000000000853 ) ) ;
#16544 = CARTESIAN_POINT ( 'NONE',  ( 0.8561741729129472844, 61.93301270000000613, 45.80000000109246372 ) ) ;
#16545 = VERTEX_POINT ( 'NONE', #2213 ) ;
#16546 = EDGE_LOOP ( 'NONE', ( #3500, #6082, #14244, #4419 ) ) ;
#16547 = EDGE_CURVE ( 'NONE', #184, #10051, #12690, .T. ) ;
#16548 = EDGE_CURVE ( 'NONE', #6405, #13224, #5266, .T. ) ;
#16549 = VECTOR ( 'NONE', #11592, 1000.000000000000000 ) ;
#16550 = CARTESIAN_POINT ( 'NONE',  ( -1.035533905932738863, 61.50000000000000000, 46.14999999999999858 ) ) ;
#16551 = DIRECTION ( 'NONE',  ( -1.156482317317871478E-16, 1.000000000000000000, 0.000000000000000000 ) ) ;
#16552 = ORIENTED_EDGE ( 'NONE', *, *, #14337, .T. ) ;
#16553 = CARTESIAN_POINT ( 'NONE',  ( -11.71628366038622104, -21.20848088107547014, 1.651559915991179495E-16 ) ) ;
#16554 = DIRECTION ( 'NONE',  ( 0.000000000000000000, -1.000000000000000000, 0.000000000000000000 ) ) ;
#16555 = EDGE_CURVE ( 'NONE', #6193, #1050, #15257, .T. ) ;
#16556 = CARTESIAN_POINT ( 'NONE',  ( -2.066987300000001415, 63.14382582708705627, 49.00000000109246656 ) ) ;
#16557 = CARTESIAN_POINT ( 'NONE',  ( -41.00000000000000711, 110.0000000000000000, -18.00000000000000355 ) ) ;
#16558 = EDGE_CURVE ( 'NONE', #12791, #11, #3391, .T. ) ;
#16559 = VECTOR ( 'NONE', #5175, 1000.000000000000000 ) ;
#16560 = CARTESIAN_POINT ( 'NONE',  ( 1.300000000000000044, -1.108512516844082141, -0.6399999999999991251 ) ) ;
#16561 = ORIENTED_EDGE ( 'NONE', *, *, #19355, .F. ) ;
#16563 = ORIENTED_EDGE ( 'NONE', *, *, #11372, .T. ) ;
#16562 = VERTEX_POINT ( 'NONE', #1932 ) ;
#16564 = CARTESIAN_POINT ( 'NONE',  ( -7.955834737091916686, -22.28918265808470522, 10.60742750791695599 ) ) ;
#16565 = AXIS2_PLACEMENT_3D ( 'NONE', #8199, #5728, #4460 ) ;
#16566 = CARTESIAN_POINT ( 'NONE',  ( -14.99999999999999645, 73.00000000000001421, 23.99999999999997868 ) ) ;
#16567 = ORIENTED_EDGE ( 'NONE', *, *, #1267, .F. ) ;
#16568 = ORIENTED_EDGE ( 'NONE', *, *, #17296, .T. ) ;
#16569 = CARTESIAN_POINT ( 'NONE',  ( -15.96867458239599635, -21.04416526290806999, 16.51757249208304046 ) ) ;
#16570 = ADVANCED_FACE ( 'NONE', ( #7915 ), #454, .F. ) ;
#16571 = CARTESIAN_POINT ( 'NONE',  ( -2.066987300000000971, 63.14382582708704916, 48.00000000109246656 ) ) ;
#16572 = LINE ( 'NONE', #3240, #16913 ) ;
#16573 = ORIENTED_EDGE ( 'NONE', *, *, #10597, .T. ) ;
#16574 = CARTESIAN_POINT ( 'NONE',  ( -12.04416526290807887, -24.96867458239596260, 21.54492750791695954 ) ) ;
#16575 = CIRCLE ( 'NONE', #12172, 1.678500596222258556 ) ;
#16576 = CARTESIAN_POINT ( 'NONE',  ( 4.000000000000000888, 47.00000000000000711, 30.00000000000000000 ) ) ;
#16577 = ORIENTED_EDGE ( 'NONE', *, *, #11078, .F. ) ;
#16578 = CARTESIAN_POINT ( 'NONE',  ( -0.1250000000000104083, 33.66708332270461312, 52.46464466094069934 ) ) ;
#16579 = ORIENTED_EDGE ( 'NONE', *, *, #303, .T. ) ;
#16580 = EDGE_CURVE ( 'NONE', #1832, #11, #3492, .T. ) ;
#16581 = LINE ( 'NONE', #10777, #9099 ) ;
#16582 = DIRECTION ( 'NONE',  ( -0.000000000000000000, -0.000000000000000000, -1.000000000000000000 ) ) ;
#16583 = VECTOR ( 'NONE', #8265, 1000.000000000000000 ) ;
#16584 = DIRECTION ( 'NONE',  ( 1.000000000000000000, 0.000000000000000000, 0.000000000000000000 ) ) ;
#16585 = VECTOR ( 'NONE', #9792, 1000.000000000000000 ) ;
#16586 = DIRECTION ( 'NONE',  ( 0.000000000000000000, 0.000000000000000000, -1.000000000000000000 ) ) ;
#16587 = CARTESIAN_POINT ( 'NONE',  ( 2.499999999999992895, 65.03553390593275196, 48.15000000218495302 ) ) ;
#16588 = CARTESIAN_POINT ( 'NONE',  ( -20.04416526290808065, -25.17491895705300209, 34.23242750791695954 ) ) ;
#16589 = DIRECTION ( 'NONE',  ( -0.000000000000000000, -0.000000000000000000, -1.000000000000000000 ) ) ;
#16590 = CARTESIAN_POINT ( 'NONE',  ( -11.46040770435012668, -27.78091578003887463, 11.48242750791695954 ) ) ;
#16591 = LINE ( 'NONE', #19238, #9896 ) ;
#16592 = EDGE_CURVE ( 'NONE', #3058, #6376, #11259, .T. ) ;
#16593 = ORIENTED_EDGE ( 'NONE', *, *, #7567, .F. ) ;
#16594 = EDGE_CURVE ( 'NONE', #15997, #17726, #4061, .T. ) ;
#16595 = CARTESIAN_POINT ( 'NONE',  ( -13.49542703274174116, -28.95583473709188738, 24.39257249208303335 ) ) ;
#16596 = EDGE_CURVE ( 'NONE', #11135, #5165, #5537, .T. ) ;
#16597 = VECTOR ( 'NONE', #9169, 999.9999999999998863 ) ;
#16598 = CARTESIAN_POINT ( 'NONE',  ( -1.040834085586084257E-14, 25.64142135623728080, 60.84386001800126564 ) ) ;
#16599 = EDGE_CURVE ( 'NONE', #5689, #2281, #13734, .T. ) ;
#16600 = CARTESIAN_POINT ( 'NONE',  ( -15.16482700510262482, -20.99999999999997513, 21.98632249208304046 ) ) ;
#16601 = DIRECTION ( 'NONE',  ( 0.000000000000000000, 0.000000000000000000, 1.000000000000000000 ) ) ;
#16602 = ORIENTED_EDGE ( 'NONE', *, *, #5806, .F. ) ;
#16603 = VECTOR ( 'NONE', #4199, 1000.000000000000000 ) ;
#16604 = LINE ( 'NONE', #5914, #13442 ) ;
#16605 = ORIENTED_EDGE ( 'NONE', *, *, #4606, .T. ) ;
#16606 = CARTESIAN_POINT ( 'NONE',  ( 2.500000000000000000, 0.000000000000000000, 0.000000000000000000 ) ) ;
#16607 = DIRECTION ( 'NONE',  ( -7.304098846218135653E-17, 0.000000000000000000, 1.000000000000000000 ) ) ;
#16608 = DIRECTION ( 'NONE',  ( 1.000000000000000000, 0.000000000000000000, 0.000000000000000000 ) ) ;
#16609 = AXIS2_PLACEMENT_3D ( 'NONE', #10654, #9381, #5090 ) ;
#16610 = CARTESIAN_POINT ( 'NONE',  ( -2.066987300000001415, 64.00000000000000000, 48.15000000109247225 ) ) ;
#16611 = CIRCLE ( 'NONE', #8165, 2.041999999999999815 ) ;
#16612 = ADVANCED_FACE ( 'NONE', ( #18968 ), #16027, .F. ) ;
#16613 = LINE ( 'NONE', #3179, #12945 ) ;
#16614 = CARTESIAN_POINT ( 'NONE',  ( -41.00000000000000711, 110.0000000000000000, 14.50000000000000000 ) ) ;
#16615 = DIRECTION ( 'NONE',  ( 0.000000000000000000, 0.000000000000000000, 1.000000000000000000 ) ) ;
#16616 = AXIS2_PLACEMENT_3D ( 'NONE', #14140, #18375, #16797 ) ;
#16617 = ORIENTED_EDGE ( 'NONE', *, *, #2905, .F. ) ;
#16618 = DIRECTION ( 'NONE',  ( 1.000000000000000000, 0.000000000000000000, 0.000000000000000000 ) ) ;
#16619 = VECTOR ( 'NONE', #18059, 1000.000000000000000 ) ;
#16620 = CARTESIAN_POINT ( 'NONE',  ( -20.04416526290808065, -25.17491895705300209, 23.73242750791694888 ) ) ;
#16621 = CARTESIAN_POINT ( 'NONE',  ( -12.64274437364855252, -28.41254052147347053, 11.70117750791695777 ) ) ;
#16622 = CARTESIAN_POINT ( 'NONE',  ( 2.500000000000001776, 64.00000000000000000, 48.90000000218494591 ) ) ;
#16623 = CARTESIAN_POINT ( 'NONE',  ( -16.50457296725825174, -19.04416526290807354, 21.76757249208304401 ) ) ;
#16624 = AXIS2_PLACEMENT_3D ( 'NONE', #1368, #7337, #14892 ) ;
#16625 = CARTESIAN_POINT ( 'NONE',  ( 0.8561741729129472844, 61.93301270000000613, 46.80000000109246372 ) ) ;
#16626 = CARTESIAN_POINT ( 'NONE',  ( -16.50457296725820555, -28.95583473709189448, 1.857427507916957765 ) ) ;
#16627 = DIRECTION ( 'NONE',  ( 0.000000000000000000, -0.7071067811865495711, 0.7071067811865454633 ) ) ;
#16628 = CARTESIAN_POINT ( 'NONE',  ( -15.16482700510259640, -28.99999999999998224, 12.13867750791695777 ) ) ;
#16629 = LINE ( 'NONE', #11705, #19373 ) ;
#16630 = CARTESIAN_POINT ( 'NONE',  ( 2.500000000000001776, 65.03553390593273775, 45.64999999999999858 ) ) ;
#16631 = AXIS2_PLACEMENT_3D ( 'NONE', #6846, #12729, #18725 ) ;
#16632 = CARTESIAN_POINT ( 'NONE',  ( -0.8561741729129465073, 61.93301270000000613, 48.30000000109247082 ) ) ;
#16633 = FACE_OUTER_BOUND ( 'NONE', #19030, .T. ) ;
#16634 = CARTESIAN_POINT ( 'NONE',  ( -41.00000000000000711, 110.0000000000000000, -25.50000000000000000 ) ) ;
#16635 = VECTOR ( 'NONE', #6975, 1000.000000000000000 ) ;
#16636 = EDGE_CURVE ( 'NONE', #5403, #18922, #6908, .T. ) ;
#16637 = FACE_OUTER_BOUND ( 'NONE', #11649, .T. ) ;
#16638 = DIRECTION ( 'NONE',  ( -0.000000000000000000, 1.000000000000000000, -0.000000000000000000 ) ) ;
#16639 = DIRECTION ( 'NONE',  ( 1.000000000000000000, 0.000000000000000000, -7.709882115452476934E-17 ) ) ;
#16640 = COLOUR_RGB ( '', 0.09019608, 0.27058824, 0.51372549) ;
#16641 = CARTESIAN_POINT ( 'NONE',  ( -50.00000000000001421, 0.000000000000000000, 59.99999999999997868 ) ) ;
#16642 = VERTEX_POINT ( 'NONE', #19162 ) ;
#16643 = ORIENTED_EDGE ( 'NONE', *, *, #18834, .T. ) ;
#16644 = CARTESIAN_POINT ( 'NONE',  ( -11.64274437364859693, -17.85540867095757989, 17.17382249208304046 ) ) ;
#16645 = VECTOR ( 'NONE', #3798, 1000.000000000000114 ) ;
#16646 = CARTESIAN_POINT ( 'NONE',  ( -10.75228648362912232, -21.35725562635138530, 17.61132249208304401 ) ) ;
#16648 = ORIENTED_EDGE ( 'NONE', *, *, #10580, .F. ) ;
#16647 = ORIENTED_EDGE ( 'NONE', *, *, #13456, .F. ) ;
#16649 = CARTESIAN_POINT ( 'NONE',  ( -15.16482700510260706, -26.99999999999998579, 17.38867750791695954 ) ) ;
#16650 = DIRECTION ( 'NONE',  ( -0.000000000000000000, 0.000000000000000000, 1.000000000000000000 ) ) ;
#16651 = CARTESIAN_POINT ( 'NONE',  ( -22.04416526290809486, -22.28918265808477628, 10.39257249208303691 ) ) ;
#16652 = AXIS2_PLACEMENT_3D ( 'NONE', #4874, #3490, #12309 ) ;
#16653 = DIRECTION ( 'NONE',  ( -0.000000000000000000, -1.000000000000000000, -0.000000000000000000 ) ) ;
#16654 = CARTESIAN_POINT ( 'NONE',  ( 1.461580736456473906, 62.53841926354353120, 45.85000000109246798 ) ) ;
#16655 = ORIENTED_EDGE ( 'NONE', *, *, #9621, .T. ) ;
#16656 = ORIENTED_EDGE ( 'NONE', *, *, #7318, .T. ) ;
#16657 = CARTESIAN_POINT ( 'NONE',  ( 4.189607678530260948, 26.72836399182260791, 59.40336399182267257 ) ) ;
#16658 = ORIENTED_EDGE ( 'NONE', *, *, #7786, .F. ) ;
#16659 = EDGE_LOOP ( 'NONE', ( #16747, #13715, #1974, #15579, #11423, #5660, #3694 ) ) ;
#16660 = CARTESIAN_POINT ( 'NONE',  ( -0.8561741729129461742, 66.06698730000000808, 48.60000000109246798 ) ) ;
#16661 = CARTESIAN_POINT ( 'NONE',  ( 0.000000000000000000, 2.357898499370431722, -2.818925648462311528E-15 ) ) ;
#16662 = CARTESIAN_POINT ( 'NONE',  ( 0.8561741729129472844, 61.93301270000000613, 48.40000000109247225 ) ) ;
#16663 = DIRECTION ( 'NONE',  ( -0.7071067811865437980, 0.5000000000000039968, -0.5000000000000013323 ) ) ;
#16664 = CARTESIAN_POINT ( 'NONE',  ( 1.767766952966369987, 65.76776695296638309, 47.40000000218494591 ) ) ;
#16665 = ORIENTED_EDGE ( 'NONE', *, *, #5921, .F. ) ;
#16667 = ORIENTED_EDGE ( 'NONE', *, *, #18796, .T. ) ;
#16666 = ORIENTED_EDGE ( 'NONE', *, *, #11425, .T. ) ;
#16668 = CARTESIAN_POINT ( 'NONE',  ( -8.044165262908075320, -26.04047135212042718, 11.04492750791695777 ) ) ;
#16669 =( BOUNDED_CURVE ( )  B_SPLINE_CURVE ( 2, ( #1787, #220, #3054, #15120, #13337, #5902, #13540, #10397, #4834 ),
 .UNSPECIFIED., .F., .F. ) 
 B_SPLINE_CURVE_WITH_KNOTS ( ( 3, 2, 2, 2, 3 ),
 ( 0.2857142857142853098, 0.3035714285714282701, 0.3214285714285712858, 0.3392857142857143016, 0.3571428571428572618 ),
 .UNSPECIFIED. ) 
 CURVE ( )  GEOMETRIC_REPRESENTATION_ITEM ( )  RATIONAL_B_SPLINE_CURVE ( ( 1.000000000000001554, 0.9238795325112850731, 1.000000000000000000, 0.9238795325112867385, 1.000000000000000000, 0.9238795325112867385, 1.000000000000000000, 0.9238795325112862944, 1.000000000000000444 ) ) 
 REPRESENTATION_ITEM ( '' )  );
#16670 = AXIS2_PLACEMENT_3D ( 'NONE', #9934, #11502, #19068 ) ;
#16671 = DIRECTION ( 'NONE',  ( -1.000000000000000000, 0.000000000000000000, -2.081668171172167774E-16 ) ) ;
#16672 = ORIENTED_EDGE ( 'NONE', *, *, #18284, .F. ) ;
#16673 = ORIENTED_EDGE ( 'NONE', *, *, #632, .T. ) ;
#16674 = CARTESIAN_POINT ( 'NONE',  ( -17.31681416490117087, -21.92450931948788551, 21.33007249208304401 ) ) ;
#16675 = CARTESIAN_POINT ( 'NONE',  ( -13.28918265808472299, -31.04416526290805933, 6.669927507916955989 ) ) ;
#16676 = DIRECTION ( 'NONE',  ( 9.251858538542970348E-17, 0.000000000000000000, -1.000000000000000000 ) ) ;
#16677 = DIRECTION ( 'NONE',  ( 0.000000000000000000, 0.000000000000000000, 1.000000000000000000 ) ) ;
#16678 = ORIENTED_EDGE ( 'NONE', *, *, #6802, .F. ) ;
#16679 = CARTESIAN_POINT ( 'NONE',  ( -15.16482700510260706, -26.99999999999998579, 17.38867750791695954 ) ) ;
#16680 = EDGE_CURVE ( 'NONE', #6552, #14552, #831, .T. ) ;
#16681 = ORIENTED_EDGE ( 'NONE', *, *, #1195, .T. ) ;
#16682 = CARTESIAN_POINT ( 'NONE',  ( -1.767766952966369765, 62.23223304703363112, 45.29999999999999005 ) ) ;
#16683 = VERTEX_POINT ( 'NONE', #3968 ) ;
#16684 = FILL_AREA_STYLE ('',( #3351 ) ) ;
#16685 = CARTESIAN_POINT ( 'NONE',  ( -1.767766952966370209, 65.76776695296638309, 46.69999999999999574 ) ) ;
#16686 = FACE_OUTER_BOUND ( 'NONE', #13154, .T. ) ;
#16687 = CARTESIAN_POINT ( 'NONE',  ( -0.1250000000000104083, 33.84290755733280776, 52.64142146683631296 ) ) ;
#16688 = CONTEXT_DEPENDENT_SHAPE_REPRESENTATION ( #2418, #4430 ) ;
#16689 = CARTESIAN_POINT ( 'NONE',  ( -15.00000000000000000, -16.78846153846157918, -16.05769230769231015 ) ) ;
#16690 = DIRECTION ( 'NONE',  ( -0.000000000000000000, -1.000000000000000000, -0.000000000000000000 ) ) ;
#16691 = CARTESIAN_POINT ( 'NONE',  ( -16.50457296725820555, -28.95583473709189448, 38.60742750791694533 ) ) ;
#16692 = LINE ( 'NONE', #7771, #17393 ) ;
#16693 = ORIENTED_EDGE ( 'NONE', *, *, #13083, .T. ) ;
#16694 = EDGE_CURVE ( 'NONE', #184, #9810, #12880, .T. ) ;
#16695 = CARTESIAN_POINT ( 'NONE',  ( -13.49542703274178379, -19.04416526290806289, 20.23242750791696309 ) ) ;
#16696 = CARTESIAN_POINT ( 'NONE',  ( 2.500000000000001776, 64.00000000000000000, 49.99999999999999289 ) ) ;
#16697 = VERTEX_POINT ( 'NONE', #18879 ) ;
#16698 = CARTESIAN_POINT ( 'NONE',  ( -10.75228648362912232, -21.35725562635138530, 12.36132249208304046 ) ) ;
#16699 = LINE ( 'NONE', #3265, #3514 ) ;
#16700 = CARTESIAN_POINT ( 'NONE',  ( -16.35725562635141372, -26.68048971390461332, 14.54882249208304401 ) ) ;
#16701 = CARTESIAN_POINT ( 'NONE',  ( -45.00000000000000000, 3.000000000000000000, 56.59999999999998010 ) ) ;
#16702 = ORIENTED_EDGE ( 'NONE', *, *, #6984, .F. ) ;
#16703 = DIRECTION ( 'NONE',  ( -4.081702296416016490E-16, 0.000000000000000000, -1.000000000000000000 ) ) ;
#16704 = VERTEX_POINT ( 'NONE', #6813 ) ;
#16705 = DIRECTION ( 'NONE',  ( 0.7071067811865463515, -0.000000000000000000, 0.7071067811865487940 ) ) ;
#16706 = CARTESIAN_POINT ( 'NONE',  ( -3.065533689247737392, -43.60761626555502346, 3.000000000000000000 ) ) ;
#16707 = LINE ( 'NONE', #10511, #4417 ) ;
#16708 = ADVANCED_FACE ( 'NONE', ( #1119 ), #8288, .F. ) ;
#16709 = ADVANCED_FACE ( 'NONE', ( #14260 ), #5632, .F. ) ;
#16710 = LINE ( 'NONE', #8084, #17519 ) ;
#16711 = EDGE_CURVE ( 'NONE', #1741, #5915, #10218, .T. ) ;
#16712 = CARTESIAN_POINT ( 'NONE',  ( -8.528048594804062077, -45.28611686177728046, 1.500000000000000000 ) ) ;
#16713 = DIRECTION ( 'NONE',  ( 0.000000000000000000, 0.000000000000000000, 1.000000000000000000 ) ) ;
#16714 = UNCERTAINTY_MEASURE_WITH_UNIT (LENGTH_MEASURE( 1.000000000000000082E-05 ), #12339, 'distance_accuracy_value', 'NONE');
#16715 = ORIENTED_EDGE ( 'NONE', *, *, #3059, .T. ) ;
#16716 = DIRECTION ( 'NONE',  ( 0.000000000000000000, 0.000000000000000000, 1.000000000000000000 ) ) ;
#16717 = CARTESIAN_POINT ( 'NONE',  ( -16.17491895705301275, -18.95583473709189803, 14.54492750791695421 ) ) ;
#16718 = CARTESIAN_POINT ( 'NONE',  ( -1.530808498934192803E-16, 66.50000000000000000, 46.70000000218494307 ) ) ;
#16719 = CARTESIAN_POINT ( 'NONE',  ( -19.99999999999999645, -24.16482700510261949, 25.92382249208304401 ) ) ;
#16720 = CARTESIAN_POINT ( 'NONE',  ( 1.461580736456473684, 65.46158073645646880, 46.25000000109246656 ) ) ;
#16721 = EDGE_CURVE ( 'NONE', #11533, #853, #16117, .T. ) ;
#16722 = CARTESIAN_POINT ( 'NONE',  ( -17.64274437364855430, -28.24771351637087236, 12.57617750791695777 ) ) ;
#16723 =( REPRESENTATION_RELATIONSHIP ('NONE','NONE', #7912, #8522 ) REPRESENTATION_RELATIONSHIP_WITH_TRANSFORMATION ( #4929 )SHAPE_REPRESENTATION_RELATIONSHIP( ) );
#16724 = CARTESIAN_POINT ( 'NONE',  ( -2.500000000000001776, 64.00000000000000000, 46.79999999999999716 ) ) ;
#16725 = CARTESIAN_POINT ( 'NONE',  ( -16.17491895705301275, -18.95583473709189448, 19.79492750791695954 ) ) ;
#16726 = DIRECTION ( 'NONE',  ( 0.000000000000000000, -1.000000000000000000, 0.000000000000000000 ) ) ;
#16727 = CARTESIAN_POINT ( 'NONE',  ( -1.530808498934192803E-16, 66.50000000000000000, 45.79999999999999005 ) ) ;
#16728 = EDGE_CURVE ( 'NONE', #12574, #9967, #7192, .T. ) ;
#16729 = CARTESIAN_POINT ( 'NONE',  ( 1.461580736456473906, 62.53841926354353120, 48.45000000109246940 ) ) ;
#16730 = LINE ( 'NONE', #12308, #6226 ) ;
#16731 = CARTESIAN_POINT ( 'NONE',  ( 2.315774708385922587, 27.80336399182260720, 58.32836399182267684 ) ) ;
#16732 = CARTESIAN_POINT ( 'NONE',  ( -1.752307227213768082, 62.82914575430081783, 45.02598915381526012 ) ) ;
#16733 = CARTESIAN_POINT ( 'NONE',  ( -0.8561741729129461742, 66.06698729999999387, 46.40000000109246514 ) ) ;
#16734 = DIRECTION ( 'NONE',  ( 0.000000000000000000, 0.000000000000000000, 1.000000000000000000 ) ) ;
#16735 = AXIS2_PLACEMENT_3D ( 'NONE', #16093, #14523, #11378 ) ;
#16736 = ORIENTED_EDGE ( 'NONE', *, *, #11271, .F. ) ;
#16737 = ORIENTED_EDGE ( 'NONE', *, *, #12173, .T. ) ;
#16738 = CARTESIAN_POINT ( 'NONE',  ( -7.955834737091903364, -25.71081734191518464, 28.76757249208303691 ) ) ;
#16739 = FILL_AREA_STYLE ('',( #6354 ) ) ;
#16740 = CARTESIAN_POINT ( 'NONE',  ( -19.99999999999999645, -24.16482700510261949, 4.923822492083040459 ) ) ;
#16741 = VERTEX_POINT ( 'NONE', #5733 ) ;
#16742 = CARTESIAN_POINT ( 'NONE',  ( -15.63902057219076269, -20.95583473709189448, 19.79492750791695954 ) ) ;
#16743 = CARTESIAN_POINT ( 'NONE',  ( 1.767766952966370653, 62.23223304703363112, 48.80000000218494449 ) ) ;
#16744 = CARTESIAN_POINT ( 'NONE',  ( -20.24501739517669563, -18.99630608921239627, 16.08007249208304046 ) ) ;
#16745 = CARTESIAN_POINT ( 'NONE',  ( -0.8561741729129461742, 66.06698729999999387, 48.60000000109246798 ) ) ;
#16746 = CARTESIAN_POINT ( 'NONE',  ( 0.8561741729129460632, 66.06698729999999387, 45.30000000109247082 ) ) ;
#16747 = ORIENTED_EDGE ( 'NONE', *, *, #17551, .F. ) ;
#16748 = EDGE_CURVE ( 'NONE', #3909, #5783, #17215, .T. ) ;
#16749 = EDGE_LOOP ( 'NONE', ( #14185, #15393, #14132, #1421 ) ) ;
#16750 = CARTESIAN_POINT ( 'NONE',  ( 2.500000000000001776, 64.00000000000000000, 45.70000000218494307 ) ) ;
#16751 = CARTESIAN_POINT ( 'NONE',  ( 44.99999999999997158, 3.000000000000000000, 53.50000000000000000 ) ) ;
#16752 = VECTOR ( 'NONE', #13951, 1000.000000000000000 ) ;
#16753 = ORIENTED_EDGE ( 'NONE', *, *, #10824, .T. ) ;
#16754 = DIRECTION ( 'NONE',  ( -0.7071067811865487940, 0.000000000000000000, 0.7071067811865462405 ) ) ;
#16755 = LINE ( 'NONE', #1559, #17500 ) ;
#16756 = CARTESIAN_POINT ( 'NONE',  ( 1.461580736456473684, 65.46158073645646880, 45.45000000109246940 ) ) ;
#16757 = EDGE_CURVE ( 'NONE', #15535, #262, #2395, .T. ) ;
#16758 = DIRECTION ( 'NONE',  ( 1.000000000000000000, -0.000000000000000000, -0.000000000000000000 ) ) ;
#16759 = CARTESIAN_POINT ( 'NONE',  ( -4.012830983233618198, 32.52836399182267257, 53.60336399182263989 ) ) ;
#16760 = EDGE_LOOP ( 'NONE', ( #5039, #6412, #3129, #11730 ) ) ;
#16762 = VERTEX_POINT ( 'NONE', #11794 ) ;
#16761 = EDGE_LOOP ( 'NONE', ( #7782, #8699, #19100, #2347, #14457 ) ) ;
#16763 = CARTESIAN_POINT ( 'NONE',  ( -14.83517299489740715, -16.99999999999997868, 9.513677507916955989 ) ) ;
#16764 = COLOUR_RGB ( '', 0.09019608, 0.27058824, 0.51372549) ;
#16765 = VERTEX_POINT ( 'NONE', #17786 ) ;
#16766 = VECTOR ( 'NONE', #15411, 1000.000000000000000 ) ;
#16767 = VERTEX_POINT ( 'NONE', #4558 ) ;
#16768 = CARTESIAN_POINT ( 'NONE',  ( -15.63902057219073605, -27.04416526290807710, 19.58007249208304046 ) ) ;
#16769 = CARTESIAN_POINT ( 'NONE',  ( -14.83517299489740715, -16.99999999999997868, 20.01367750791695954 ) ) ;
#16770 = CARTESIAN_POINT ( 'NONE',  ( 1.461580736456473684, 65.46158073645646880, 48.45000000109247651 ) ) ;
#16771 = CARTESIAN_POINT ( 'NONE',  ( 2.500000000000001776, 64.00000000000000000, 48.90000000218494591 ) ) ;
#16772 = EDGE_CURVE ( 'NONE', #9140, #14781, #19235, .T. ) ;
#16773 = ORIENTED_EDGE ( 'NONE', *, *, #2886, .F. ) ;
#16774 = CARTESIAN_POINT ( 'NONE',  ( -12.68318583509884157, -21.92450931948787485, 15.41992750791695954 ) ) ;
#16775 = EDGE_LOOP ( 'NONE', ( #10201, #16059, #15205, #11950 ) ) ;
#16776 = PLANE ( 'NONE',  #1895 ) ;
#16777 = ORIENTED_EDGE ( 'NONE', *, *, #11271, .T. ) ;
#16778 = CYLINDRICAL_SURFACE ( 'NONE', #1298, 1.599999999999997202 ) ;
#16779 = DIRECTION ( 'NONE',  ( -0.000000000000000000, -0.000000000000000000, -1.000000000000000000 ) ) ;
#16780 = FACE_BOUND ( 'NONE', #6225, .T. ) ;
#16781 = DIRECTION ( 'NONE',  ( 0.000000000000000000, 0.000000000000000000, 1.000000000000000000 ) ) ;
#16782 = AXIS2_PLACEMENT_3D ( 'NONE', #13115, #7540, #7439 ) ;
#16783 = CARTESIAN_POINT ( 'NONE',  ( -0.8561741729129461742, 66.06698729999999387, 48.60000000109246798 ) ) ;
#16784 = CIRCLE ( 'NONE', #3618, 1.500000000000001332 ) ;
#16785 = DIRECTION ( 'NONE',  ( -1.000000000000000000, 0.000000000000000000, -0.000000000000000000 ) ) ;
#16786 = CARTESIAN_POINT ( 'NONE',  ( 1.035533905932739751, 61.50000000000000000, 46.35000000218494165 ) ) ;
#16787 = LINE ( 'NONE', #14824, #9897 ) ;
#16788 = DIRECTION ( 'NONE',  ( -1.000000000000000000, -0.000000000000000000, -0.000000000000000000 ) ) ;
#16789 = VERTEX_POINT ( 'NONE', #19356 ) ;
#16790 = CARTESIAN_POINT ( 'NONE',  ( -20.04416526290808065, -25.17491895705300209, 18.48242750791695954 ) ) ;
#16791 = DIRECTION ( 'NONE',  ( 0.000000000000000000, 0.000000000000000000, 1.000000000000000000 ) ) ;
#16792 = VERTEX_POINT ( 'NONE', #7486 ) ;
#16793 = CARTESIAN_POINT ( 'NONE',  ( -9.955834737091903364, -25.17491895705294880, 13.01757249208304223 ) ) ;
#16794 = AXIS2_PLACEMENT_3D ( 'NONE', #18107, #10542, #12585 ) ;
#16795 = VECTOR ( 'NONE', #11030, 1000.000000000000000 ) ;
#16796 = CARTESIAN_POINT ( 'NONE',  ( -12.04416526290808420, -23.03132541760398766, 12.58007249208304401 ) ) ;
#16797 = DIRECTION ( 'NONE',  ( 0.000000000000000000, 0.000000000000000000, 1.000000000000000000 ) ) ;
#16798 = ORIENTED_EDGE ( 'NONE', *, *, #6494, .F. ) ;
#16799 = CARTESIAN_POINT ( 'NONE',  ( -24.00000000000000000, 110.0000000000000000, 13.50000000000000178 ) ) ;
#16800 = ORIENTED_EDGE ( 'NONE', *, *, #10934, .T. ) ;
#16801 = FACE_BOUND ( 'NONE', #15576, .T. ) ;
#16802 = EDGE_CURVE ( 'NONE', #7943, #4327, #10516, .T. ) ;
#16803 = ADVANCED_FACE ( 'NONE', ( #11692, #2881, #16411 ), #11989, .T. ) ;
#16804 = CARTESIAN_POINT ( 'NONE',  ( 41.00000000000000000, 47.00000000000000711, 18.00000000000000000 ) ) ;
#16805 = DIRECTION ( 'NONE',  ( 0.000000000000000000, 1.224646799147353207E-16, 1.000000000000000000 ) ) ;
#16806 = CARTESIAN_POINT ( 'NONE',  ( -1.461580736456473906, 65.46158073645646880, 44.85000000109246798 ) ) ;
#16807 = ADVANCED_FACE ( 'NONE', ( #5925 ), #1707, .T. ) ;
#16808 = VECTOR ( 'NONE', #2568, 1000.000000000000000 ) ;
#16809 = AXIS2_PLACEMENT_3D ( 'NONE', #12479, #3853, #5424 ) ;
#16810 = CARTESIAN_POINT ( 'NONE',  ( -1.035533905932738641, 66.50000000000000000, 45.04999999999999005 ) ) ;
#16811 = DIRECTION ( 'NONE',  ( 0.000000000000000000, 0.000000000000000000, -1.000000000000000000 ) ) ;
#16812 = ORIENTED_EDGE ( 'NONE', *, *, #4129, .T. ) ;
#16813 = DIRECTION ( 'NONE',  ( 0.000000000000000000, 0.000000000000000000, 1.000000000000000000 ) ) ;
#16814 = CARTESIAN_POINT ( 'NONE',  ( -13.49542703274178379, -19.04416526290806289, 20.23242750791696309 ) ) ;
#16815 = EDGE_CURVE ( 'NONE', #4659, #7863, #5831, .T. ) ;
#16816 = CARTESIAN_POINT ( 'NONE',  ( -1.035533905932738863, 61.50000000000000000, 45.45000000218495018 ) ) ;
#16817 = ADVANCED_FACE ( 'NONE', ( #16211 ), #1322, .F. ) ;
#16818 = CARTESIAN_POINT ( 'NONE',  ( -16.17491895705296656, -29.04416526290807710, 14.33007249208304046 ) ) ;
#16819 = VECTOR ( 'NONE', #13023, 1000.000000000000000 ) ;
#16820 = DIRECTION ( 'NONE',  ( -1.000000000000000000, 0.000000000000000000, -0.000000000000000000 ) ) ;
#16821 = CARTESIAN_POINT ( 'NONE',  ( -13.82508104294698192, -29.04416526290806644, 22.41992750791695244 ) ) ;
#16822 = CARTESIAN_POINT ( 'NONE',  ( -1.485306817036799787, 0.000000000000000000, 7.999999999999996447 ) ) ;
#16823 = CARTESIAN_POINT ( 'NONE',  ( -18.78091578003889595, -27.53959229564985023, 12.79492750791695599 ) ) ;
#16824 = FACE_OUTER_BOUND ( 'NONE', #11053, .T. ) ;
#16825 = DIRECTION ( 'NONE',  ( -1.000000000000000000, 0.000000000000000000, 0.000000000000000000 ) ) ;
#16826 = EDGE_CURVE ( 'NONE', #9848, #15994, #13655, .T. ) ;
#16827 = CARTESIAN_POINT ( 'NONE',  ( -2.066987300000001415, 63.14382582708705627, 47.40000000109247225 ) ) ;
#16828 = CARTESIAN_POINT ( 'NONE',  ( -2.500000000000001776, 64.00000000000000000, 45.19999999999999574 ) ) ;
#16829 = DIRECTION ( 'NONE',  ( 0.000000000000000000, 1.000000000000000000, 0.000000000000000000 ) ) ;
#16830 = DIRECTION ( 'NONE',  ( 0.000000000000000000, 1.000000000000000000, 0.000000000000000000 ) ) ;
#16831 = CARTESIAN_POINT ( 'NONE',  ( -1.461580736456473462, 62.53841926354353120, 48.25000000109246656 ) ) ;
#16832 = LINE ( 'NONE', #13979, #14563 ) ;
#16833 = ORIENTED_EDGE ( 'NONE', *, *, #13207, .F. ) ;
#16834 = VERTEX_POINT ( 'NONE', #10415 ) ;
#16835 = CARTESIAN_POINT ( 'NONE',  ( -18.64274437364860049, -18.02023567606023491, 32.04882249208304046 ) ) ;
#16836 = MANIFOLD_SOLID_BREP ( 'Cavity1', #12604 ) ;
#16837 = EDGE_CURVE ( 'NONE', #10481, #7135, #16613, .T. ) ;
#16838 = CARTESIAN_POINT ( 'NONE',  ( -15.16482700510263371, -18.99999999999997868, 11.48632249208304046 ) ) ;
#16840 = ORIENTED_EDGE ( 'NONE', *, *, #7360, .F. ) ;
#16839 = EDGE_CURVE ( 'NONE', #18711, #15312, #10223, .T. ) ;
#16841 = CARTESIAN_POINT ( 'NONE',  ( -12.92450931948788906, -26.31681416490114245, 27.23242750791697020 ) ) ;
#16842 = CARTESIAN_POINT ( 'NONE',  ( -40.00000000000000711, 110.0000000000000000, -11.50000000000000000 ) ) ;
#16843 = CARTESIAN_POINT ( 'NONE',  ( -9.996306089212408708, -18.75498260482328661, 22.64257249208304046 ) ) ;
#16844 = CARTESIAN_POINT ( 'NONE',  ( -1.461580736456473462, 62.53841926354353120, 47.25000000109247367 ) ) ;
#16845 = CARTESIAN_POINT ( 'NONE',  ( -2.066987300000001415, 64.00000000000000000, 47.95000000109246940 ) ) ;
#16846 = EDGE_LOOP ( 'NONE', ( #8721, #8135, #18078, #10275 ) ) ;
#16847 = ORIENTED_EDGE ( 'NONE', *, *, #10106, .F. ) ;
#16848 = EDGE_CURVE ( 'NONE', #5501, #663, #12650, .T. ) ;
#16849 = CARTESIAN_POINT ( 'NONE',  ( -24.00000000000000000, 53.00000000000000711, 30.00000000000000000 ) ) ;
#16850 = LINE ( 'NONE', #7934, #17571 ) ;
#16851 = ORIENTED_EDGE ( 'NONE', *, *, #2055, .F. ) ;
#16852 = CARTESIAN_POINT ( 'NONE',  ( -2.066987300000001415, 64.00000000000000000, 48.75000000109246656 ) ) ;
#16853 = LINE ( 'NONE', #13997, #18469 ) ;
#16854 = CARTESIAN_POINT ( 'NONE',  ( 0.8561741729129472844, 61.93301270000000613, 45.20000000109248361 ) ) ;
#16855 = DIRECTION ( 'NONE',  ( 0.000000000000000000, -0.7071067811865493491, 0.7071067811865457964 ) ) ;
#16856 = CARTESIAN_POINT ( 'NONE',  ( 1.035533905932739751, 61.50000000000000000, 45.55000000218493739 ) ) ;
#16857 = ADVANCED_FACE ( 'NONE', ( #12477 ), #3663, .T. ) ;
#16858 = ORIENTED_EDGE ( 'NONE', *, *, #1135, .T. ) ;
#16860 = ORIENTED_EDGE ( 'NONE', *, *, #17646, .T. ) ;
#16859 = ORIENTED_EDGE ( 'NONE', *, *, #15852, .F. ) ;
#16861 = CARTESIAN_POINT ( 'NONE',  ( -11.35725562635144925, -18.02023567606020293, 25.70117750791695599 ) ) ;
#16862 = CARTESIAN_POINT ( 'NONE',  ( 50.00000000000000000, 115.0000000000000000, -56.99999999999999289 ) ) ;
#16863 = ORIENTED_EDGE ( 'NONE', *, *, #18266, .F. ) ;
#16864 = ORIENTED_EDGE ( 'NONE', *, *, #5052, .T. ) ;
#16865 = CARTESIAN_POINT ( 'NONE',  ( -15.16482700510262482, -20.99999999999997513, 32.48632249208304756 ) ) ;
#16866 = CARTESIAN_POINT ( 'NONE',  ( -9.020235676060220698, -27.64274437364852588, 21.76367750791695954 ) ) ;
#16867 = CARTESIAN_POINT ( 'NONE',  ( -2.066987300000001415, 64.85617417291294373, 47.10000000109246798 ) ) ;
#16868 = DIRECTION ( 'NONE',  ( -0.000000000000000000, -0.000000000000000000, -1.000000000000000000 ) ) ;
#16869 = ORIENTED_EDGE ( 'NONE', *, *, #2594, .T. ) ;
#16870 = CARTESIAN_POINT ( 'NONE',  ( -11.95583473709191047, -23.36097942780921954, 10.60742750791695954 ) ) ;
#16871 = DIRECTION ( 'NONE',  ( -1.156482317317871478E-16, 1.000000000000000000, 0.000000000000000000 ) ) ;
#16872 = VERTEX_POINT ( 'NONE', #9446 ) ;
#16873 = CYLINDRICAL_SURFACE ( 'NONE', #14398, 1.678500596222258556 ) ;
#16874 = VERTEX_POINT ( 'NONE', #18286 ) ;
#16875 = DIRECTION ( 'NONE',  ( 1.000000000000000000, 0.000000000000000000, 0.000000000000000000 ) ) ;
#16876 = CARTESIAN_POINT ( 'NONE',  ( -40.00000000000000711, 113.0000000000000000, -18.00000000000000355 ) ) ;
#16877 = FACE_OUTER_BOUND ( 'NONE', #2945, .T. ) ;
#16878 = CARTESIAN_POINT ( 'NONE',  ( -41.00000000000000711, 110.0000000000000000, -30.99999999999999645 ) ) ;
#16879 = CARTESIAN_POINT ( 'NONE',  ( 0.000000000000000000, 0.000000000000000000, 0.000000000000000000 ) ) ;
#16880 = CARTESIAN_POINT ( 'NONE',  ( -1.461580736456473462, 62.53841926354353120, 48.05000000109247082 ) ) ;
#16881 = CARTESIAN_POINT ( 'NONE',  ( 2.500000000000007550, 65.03553390593272354, 48.95000000218495018 ) ) ;
#16882 = CYLINDRICAL_SURFACE ( 'NONE', #10642, 1.599999999999997202 ) ;
#16883 = AXIS2_PLACEMENT_3D ( 'NONE', #15036, #1206, #6393 ) ;
#16884 = FACE_OUTER_BOUND ( 'NONE', #391, .T. ) ;
#16885 = DIRECTION ( 'NONE',  ( 0.000000000000000000, -0.7071067811865492381, 0.7071067811865456854 ) ) ;
#16886 = ORIENTED_EDGE ( 'NONE', *, *, #7318, .F. ) ;
#16887 = CARTESIAN_POINT ( 'NONE',  ( -19.24771351637089367, -21.35725562635142438, 24.38867750791695954 ) ) ;
#16888 = LINE ( 'NONE', #16696, #5224 ) ;
#16889 = ORIENTED_EDGE ( 'NONE', *, *, #1242, .T. ) ;
#16890 = PRODUCT_DEFINITION_CONTEXT ( 'detailed design', #7436, 'design' ) ;
#16891 = CARTESIAN_POINT ( 'NONE',  ( -9.999999999999994671, -23.83517299489734143, 12.79882249208304046 ) ) ;
#16892 = VECTOR ( 'NONE', #9198, 1000.000000000000000 ) ;
#16893 = CARTESIAN_POINT ( 'NONE',  ( -14.03132541760400009, -26.95583473709189448, 13.89257249208304401 ) ) ;
#16894 = CARTESIAN_POINT ( 'NONE',  ( -24.00000000000000711, 53.00000000000000711, -11.50000000000000000 ) ) ;
#16895 = ORIENTED_EDGE ( 'NONE', *, *, #5203, .F. ) ;
#16896 = DIRECTION ( 'NONE',  ( 1.000000000000000000, -0.000000000000000000, -0.000000000000000000 ) ) ;
#16897 = VERTEX_POINT ( 'NONE', #4854 ) ;
#16898 = FACE_BOUND ( 'NONE', #6251, .T. ) ;
#16899 = CARTESIAN_POINT ( 'NONE',  ( -2.499999999999996003, 62.96446609406726225, 46.04999999999999005 ) ) ;
#16900 =( BOUNDED_CURVE ( )  B_SPLINE_CURVE ( 2, ( #19036, #12601, #1091, #7071, #5606, #9652, #18063, #16587, #7769 ),
 .UNSPECIFIED., .F., .F. ) 
 B_SPLINE_CURVE_WITH_KNOTS ( ( 3, 2, 2, 2, 3 ),
 ( 0.1428571428571428215, 0.1607142857142856429, 0.1785714285714284644, 0.1964285714285712858, 0.2142857142857140795 ),
 .UNSPECIFIED. ) 
 CURVE ( )  GEOMETRIC_REPRESENTATION_ITEM ( )  RATIONAL_B_SPLINE_CURVE ( ( 1.000000000000000222, 0.9238795325112866275, 1.000000000000000000, 0.9238795325112867385, 1.000000000000000000, 0.9238795325112867385, 1.000000000000000000, 0.9238795325112875156, 0.9999999999999992228 ) ) 
 REPRESENTATION_ITEM ( '' )  );
#16901 = LINE ( 'NONE', #9629, #1294 ) ;
#16902 = CARTESIAN_POINT ( 'NONE',  ( 0.000000000000000000, 3.000000000000000000, 0.000000000000000000 ) ) ;
#16903 = VECTOR ( 'NONE', #7449, 1000.000000000000000 ) ;
#16904 = CARTESIAN_POINT ( 'NONE',  ( -24.00000000000000000, 53.00000000000000711, -19.00000000000000355 ) ) ;
#16905 = CARTESIAN_POINT ( 'NONE',  ( -41.00000000000000711, 113.0000000000000000, -50.00000000000000000 ) ) ;
#16906 = LINE ( 'NONE', #6325, #9267 ) ;
#16907 = VECTOR ( 'NONE', #2280, 1000.000000000000000 ) ;
#16908 = VECTOR ( 'NONE', #14021, 1000.000000000000000 ) ;
#16909 = ORIENTED_EDGE ( 'NONE', *, *, #1469, .F. ) ;
#16910 = EDGE_CURVE ( 'NONE', #18801, #4943, #8899, .T. ) ;
#16911 = EDGE_CURVE ( 'NONE', #16046, #3132, #4953, .T. ) ;
#16912 = CARTESIAN_POINT ( 'NONE',  ( -10.75228648362910100, -26.64274437364854009, 21.76367750791695599 ) ) ;
#16913 = VECTOR ( 'NONE', #16677, 1000.000000000000000 ) ;
#16914 = CARTESIAN_POINT ( 'NONE',  ( 2.500000000000002220, 62.96446609406726935, 45.65000000218494591 ) ) ;
#16915 = EDGE_CURVE ( 'NONE', #1049, #3171, #622, .T. ) ;
#16916 = CARTESIAN_POINT ( 'NONE',  ( -18.78091578003892081, -20.46040770435013556, 21.33007249208303691 ) ) ;
#16917 = VECTOR ( 'NONE', #8222, 1000.000000000000000 ) ;
#16918 = CARTESIAN_POINT ( 'NONE',  ( -45.00000000000000000, 0.000000000000000000, 56.59999999999998010 ) ) ;
#16919 = CARTESIAN_POINT ( 'NONE',  ( -13.82508104294698192, -29.04416526290806644, 17.16992750791694888 ) ) ;
#16920 = EDGE_CURVE ( 'NONE', #7973, #19316, #5045, .T. ) ;
#16921 = PLANE ( 'NONE',  #6426 ) ;
#16922 = CARTESIAN_POINT ( 'NONE',  ( -13.82508104294698015, -29.04416526290806289, 22.41992750791695599 ) ) ;
#16923 = AXIS2_PLACEMENT_3D ( 'NONE', #13724, #5015, #3631 ) ;
#16924 = CARTESIAN_POINT ( 'NONE',  ( 14.99999999999998579, 47.00000000000000711, 23.99999999999997158 ) ) ;
#16925 = CARTESIAN_POINT ( 'NONE',  ( -12.35725562635140307, -28.24771351637085459, 29.42382249208304401 ) ) ;
#16926 = CARTESIAN_POINT ( 'NONE',  ( 2.066987300000001415, 64.00000000000000000, 47.75000000109246656 ) ) ;
#16927 = CARTESIAN_POINT ( 'NONE',  ( 44.99999999999998579, 3.000000000000000000, -54.99999999999998579 ) ) ;
#16928 = LINE ( 'NONE', #12499, #8205 ) ;
#16929 = VECTOR ( 'NONE', #6312, 1000.000000000000000 ) ;
#16930 = DIRECTION ( 'NONE',  ( 0.000000000000000000, 0.000000000000000000, -1.000000000000000000 ) ) ;
#16931 = CARTESIAN_POINT ( 'NONE',  ( -1.265664690411616068E-16, 66.06698730000000808, 48.75000000109246656 ) ) ;
#16932 = DIRECTION ( 'NONE',  ( 0.000000000000000000, 0.4999999999999991118, -0.8660254037844391517 ) ) ;
#16933 = AXIS2_PLACEMENT_3D ( 'NONE', #7226, #172, #10351 ) ;
#16934 = VERTEX_POINT ( 'NONE', #2188 ) ;
#16935 = ORIENTED_EDGE ( 'NONE', *, *, #9738, .T. ) ;
#16936 = CARTESIAN_POINT ( 'NONE',  ( -15.16482700510264436, -16.99999999999997868, 27.23632249208303691 ) ) ;
#16937 = EDGE_CURVE ( 'NONE', #8366, #3614, #11007, .T. ) ;
#16938 = MANIFOLD_SOLID_BREP ( 'Cut-Extrude-Thin1', #16008 ) ;
#16939 = CIRCLE ( 'NONE', #8470, 2.499999999999998668 ) ;
#16940 = CARTESIAN_POINT ( 'NONE',  ( -19.24771351637086880, -26.64274437364857206, 14.98632249208304046 ) ) ;
#16941 = ORIENTED_EDGE ( 'NONE', *, *, #7586, .F. ) ;
#16942 = CARTESIAN_POINT ( 'NONE',  ( -12.68318583509884157, -21.92450931948787485, 36.41992750791695954 ) ) ;
#16943 = FACE_OUTER_BOUND ( 'NONE', #4957, .T. ) ;
#16944 = CARTESIAN_POINT ( 'NONE',  ( -20.97976432393974022, -27.64274437364858628, 14.98632249208303868 ) ) ;
#16945 = VECTOR ( 'NONE', #8829, 1000.000000000000114 ) ;
#16946 = CARTESIAN_POINT ( 'NONE',  ( 0.8561741729129472844, 61.93301270000000613, 45.00000000109246656 ) ) ;
#16947 = CARTESIAN_POINT ( 'NONE',  ( -2.066987300000001859, 64.85617417291294373, 47.10000000109246798 ) ) ;
#16948 = VERTEX_POINT ( 'NONE', #8086 ) ;
#16949 = ORIENTED_EDGE ( 'NONE', *, *, #5566, .F. ) ;
#16950 = CARTESIAN_POINT ( 'NONE',  ( 14.99999999999998579, 73.00000000000001421, 23.99999999999997158 ) ) ;
#16951 = CARTESIAN_POINT ( 'NONE',  ( 43.49999999999997868, 118.0000000000000142, -52.50000000000002132 ) ) ;
#16952 = AXIS2_PLACEMENT_3D ( 'NONE', #15474, #18330, #2042 ) ;
#16953 = DIRECTION ( 'NONE',  ( 0.000000000000000000, 1.000000000000000000, 0.000000000000000000 ) ) ;
#16954 = CARTESIAN_POINT ( 'NONE',  ( -45.00000000000000000, 6.000000000000000000, 53.49999999999998579 ) ) ;
#16955 = VECTOR ( 'NONE', #14192, 1000.000000000000000 ) ;
#16956 = CARTESIAN_POINT ( 'NONE',  ( 2.066987300000001859, 64.85617417291294373, 45.40000000109246514 ) ) ;
#16957 = EDGE_CURVE ( 'NONE', #6518, #11598, #2102, .T. ) ;
#16958 = EDGE_CURVE ( 'NONE', #4628, #4224, #15330, .T. ) ;
#16959 = DIRECTION ( 'NONE',  ( 1.156482317317871478E-16, -1.000000000000000000, 0.000000000000000000 ) ) ;
#16960 = ADVANCED_FACE ( 'NONE', ( #7989 ), #6614, .T. ) ;
#16961 = CARTESIAN_POINT ( 'NONE',  ( -32.50000000000000000, 52.00000000000000711, -37.50000000000000711 ) ) ;
#16962 = ORIENTED_EDGE ( 'NONE', *, *, #15945, .F. ) ;
#16963 = ORIENTED_EDGE ( 'NONE', *, *, #1576, .F. ) ;
#16964 = CARTESIAN_POINT ( 'NONE',  ( -22.04416526290807710, -25.71081734191525925, 23.73242750791695954 ) ) ;
#16965 =( LENGTH_UNIT ( ) NAMED_UNIT ( * ) SI_UNIT ( .MILLI., .METRE. ) );
#16966 = VECTOR ( 'NONE', #2857, 1000.000000000000000 ) ;
#16967 = EDGE_LOOP ( 'NONE', ( #18820, #12518, #10441, #16121 ) ) ;
#16968 = ORIENTED_EDGE ( 'NONE', *, *, #6088, .T. ) ;
#16969 = CARTESIAN_POINT ( 'NONE',  ( -17.07549068051208963, -26.31681416490115311, 35.76757249208304756 ) ) ;
#16970 = CARTESIAN_POINT ( 'NONE',  ( -15.16482700510258574, -30.99999999999998224, 22.63867750791695954 ) ) ;
#16971 = CARTESIAN_POINT ( 'NONE',  ( 0.2500000000000002220, 0.000000000000000000, 0.000000000000000000 ) ) ;
#16972 = CARTESIAN_POINT ( 'NONE',  ( -41.00000000000000711, 110.0000000000000000, -24.49999999999999645 ) ) ;
#16973 = ORIENTED_EDGE ( 'NONE', *, *, #10118, .T. ) ;
#16974 = CARTESIAN_POINT ( 'NONE',  ( -14.03132541760401786, -21.04416526290806289, 30.73242750791696309 ) ) ;
#16975 = SURFACE_STYLE_FILL_AREA ( #4919 ) ;
#16976 = ORIENTED_EDGE ( 'NONE', *, *, #11313, .F. ) ;
#16977 = LINE ( 'NONE', #15405, #2809 ) ;
#16978 = ORIENTED_EDGE ( 'NONE', *, *, #7244, .F. ) ;
#16979 = CARTESIAN_POINT ( 'NONE',  ( -32.50000000000000000, 52.00000000000000711, 15.00000000000000000 ) ) ;
#16980 = EDGE_CURVE ( 'NONE', #232, #17355, #15238, .T. ) ;
#16981 = EDGE_CURVE ( 'NONE', #9587, #1661, #13756, .T. ) ;
#16982 = FACE_OUTER_BOUND ( 'NONE', #14300, .T. ) ;
#16983 = CARTESIAN_POINT ( 'NONE',  ( 14.33926609531033058, -43.78611686177728046, 3.000000000000000000 ) ) ;
#16984 = LINE ( 'NONE', #12453, #16766 ) ;
#16985 = CARTESIAN_POINT ( 'NONE',  ( -2.066987300000001415, 63.14382582708705627, 48.00000000109246656 ) ) ;
#16986 = VECTOR ( 'NONE', #11862, 1000.000000000000000 ) ;
#16987 = DIRECTION ( 'NONE',  ( 0.000000000000000000, -1.000000000000000000, 0.000000000000000000 ) ) ;
#16988 = DIRECTION ( 'NONE',  ( -0.000000000000000000, -0.000000000000000000, -1.000000000000000000 ) ) ;
#16989 = VECTOR ( 'NONE', #11435, 1000.000000000000000 ) ;
#16990 = CARTESIAN_POINT ( 'NONE',  ( -1.040834085586084257E-14, 27.62132034355962773, 54.62132034355965260 ) ) ;
#16991 = CARTESIAN_POINT ( 'NONE',  ( 0.000000000000000000, 0.000000000000000000, 30.00000000000000000 ) ) ;
#16992 = ORIENTED_EDGE ( 'NONE', *, *, #847, .F. ) ;
#16993 = CARTESIAN_POINT ( 'NONE',  ( -13.49542703274178379, -19.04416526290806289, 25.48242750791694888 ) ) ;
#16994 = FACE_BOUND ( 'NONE', #14996, .T. ) ;
#16995 = ORIENTED_EDGE ( 'NONE', *, *, #9041, .T. ) ;
#16996 = CARTESIAN_POINT ( 'NONE',  ( -15.16482700510263371, -18.99999999999997868, 32.48632249208304046 ) ) ;
#16997 = CARTESIAN_POINT ( 'NONE',  ( -16.35725562635141372, -26.68048971390461332, 19.79882249208304046 ) ) ;
#16998 = LINE ( 'NONE', #6409, #10009 ) ;
#16999 = ORIENTED_EDGE ( 'NONE', *, *, #11308, .F. ) ;
#17000 = CARTESIAN_POINT ( 'NONE',  ( -32.50000000000000000, 52.00000000000000711, -37.65000000000000568 ) ) ;
#17001 = VERTEX_POINT ( 'NONE', #1004 ) ;
#17002 = ADVANCED_FACE ( 'NONE', ( #18671 ), #17370, .F. ) ;
#17003 = DIRECTION ( 'NONE',  ( -1.000000000000000000, -3.826732013112563602E-16, 0.000000000000000000 ) ) ;
#17004 = CARTESIAN_POINT ( 'NONE',  ( 1.035533905932739751, 61.50000000000000000, 46.24999999999999289 ) ) ;
#17005 = DIRECTION ( 'NONE',  ( 1.000000000000000000, -0.000000000000000000, -0.000000000000000000 ) ) ;
#17006 = VECTOR ( 'NONE', #2038, 1000.000000000000000 ) ;
#17007 = CARTESIAN_POINT ( 'NONE',  ( -41.00000000000000711, 53.00000000000000711, -25.50000000000000000 ) ) ;
#17008 = CARTESIAN_POINT ( 'NONE',  ( -24.00000000000000000, 53.00000000000000711, -11.49999999999999645 ) ) ;
#17009 = LINE ( 'NONE', #4766, #15068 ) ;
#17010 = LINE ( 'NONE', #15811, #19306 ) ;
#17011 = DIRECTION ( 'NONE',  ( -0.7071067811865495711, 0.000000000000000000, -0.7071067811865455743 ) ) ;
#17012 = ORIENTED_EDGE ( 'NONE', *, *, #3097, .F. ) ;
#17013 = CARTESIAN_POINT ( 'NONE',  ( -19.41254052147348830, -26.35725562635142083, 18.26367750791695599 ) ) ;
#17014 = CARTESIAN_POINT ( 'NONE',  ( -2.500000000000000888, 62.96446609406726935, 44.55000000218495870 ) ) ;
#17015 = CARTESIAN_POINT ( 'NONE',  ( -17.35725562635140307, -28.41254052147349185, 14.54882249208304046 ) ) ;
#17016 =( BOUNDED_SURFACE ( )  B_SPLINE_SURFACE ( 3, 2, ( 
 ( #4174, #2889, #16517, #2785, #14754, #8764, #13068, #1328, #10522, #1219, #17897, #13369, #7493, #7298, #19361, #10231, #14849, #5835, #16122, #11799, #13264, #19266, #3080, #4565, #14553, #4469, #1124, #13469, #19066, #10421, #14951, #17793, #52, #4366, #1422, #7104, #10325, #1524, #16323, #19167, #8865, #5638, #8961, #5738, #7398, #4269, #5929, #2691, #16416, #2981, #17597, #8667, #7200, #13173, #3478, #9255, #10817, #13662, #1814, #244, #4860, #18090, #18293, #9346, #10619, #7597, #3379, #18389, #11014, #10723, #15242, #16717, #13563, #3284, #5054, #9161, #6425, #7901, #2005, #7794, #13865, #4773, #15337, #346, #4662, #6332, #13764, #12298, #17013, #12484, #536, #12392, #9061, #7995, #144, #4958, #9452, #16814, #13962, #1915, #441, #6519, #10914, #15440, #16912, #6228, #18485, #15049, #1627, #12193, #6130, #18194, #12092, #16620, #3187, #15145, #1713, #7696, #18581, #9640, #17376, #3764, #5334, #8189, #15730, #14157, #18762, #12589, #12766, #3858, #5147, #2107, #17292, #12864, #6620, #5427, #8091, #910, #15625, #14336, #15536, #727, #9734, #14056, #12952, #15909, #6705, #6986, #8368, #2290, #11107, #6891, #8276, #17200, #14246, #17105, #9820, #2194, #3669, #12676, #5518, #18678, #5244, #11197, #3952, #817, #6801, #18865, #629, #11296, #15816, #2383, #11385, #9914, #2471, #18951, #8461, #14437, #1011, #11480, #3570, #9543, #2666, #4720, #1399, #2866, #8647, #8554, #9210, #17769, #8845, #14529, #16100 ),
 ( #1307, #13348, #1100, #7082, #19148, #4343, #16014, #13045, #7280, #1770, #5616, #4246, #19044, #11578, #10300, #17576, #14629, #10676, #7376, #14830, #1193, #4154, #15202, #16293, #19342, #10104, #7176, #5908, #10008, #13245, #13149, #11874, #18142, #5718, #17468, #16675, #3238, #11677, #17668, #19243, #10205, #7752, #13717, #4043, #2572, #11777, #5811, #294, #6279, #16196, #2763, #8737, #14728, #6381, #9592, #397, #15486, #17057, #15396, #12250, #9308, #8137, #12632, #6475, #18628, #10766, #5195, #11153, #9497, #12343, #15293, #14009, #17151, #15678, #18342, #2056, #1963, #14110, #18247, #3712, #769, #15582, #9686, #489, #3340, #2248, #8237, #4912, #7949, #7852, #2149, #9401, #1866, #10965, #685, #8047, #16769, #3429, #6668, #580, #18438, #14204, #13912, #12442, #16866, #12539, #10871, #5007, #16970, #3530, #4819, #6573, #13818, #3622, #18540, #5107, #11061, #14293, #1053, #5384, #2337, #11342, #8692, #3901, #860, #7030, #17334, #8322, #9871, #14675, #15865, #6839, #2425, #7129, #3998, #9956, #2613, #3813, #15773, #8408, #13000, #5282, #17244, #15958, #10148, #12812, #12909, #18810, #14383, #19001, #959, #6939, #13096, #10058, #11524, #18905, #9780, #17619, #5567, #17518, #5469, #11434, #4098, #18718, #2523, #17428, #8597, #14581, #8505, #6753, #16053, #19095, #14482, #1152, #5665, #11629, #4196, #2719, #12721, #11240, #16150, #16444, #3012, #3217, #4497, #6061, #8989, #8890, #14784, #18020, #8796, #10452, #12024 ),
 ( #14878, #7628, #14976, #5863, #1452, #13592, #15080, #11823, #1549, #4397, #7525, #10253, #10357, #13499, #4595, #10553, #16242, #7325, #1654, #7425, #81, #17819, #13392, #16351, #16542, #2815, #3110, #9091, #1353, #19193, #177, #6163, #4296, #12123, #5760, #18118, #13290, #4690, #13199, #2916, #19388, #11722, #10648, #16651, #5961, #9189, #1251, #11932, #19293, #7230, #17719, #17925, #11131, #7729, #9477, #4798, #4886, #8022, #6548, #5083, #10747, #1839, #9566, #15369, #16944, #371, #7926, #6359, #10941, #16744, #4984, #15463, #3314, #13692, #2031, #11040, #18221, #17038, #268, #12514, #7823, #18515, #6254, #12322, #1943, #12220, #5170, #8113, #18318, #18606, #559, #13889, #15270, #14086, #660, #10849, #17129, #9284, #3595, #16843, #15561, #13791, #3405, #3692, #9374, #2129, #6646, #465, #6451, #3508, #12611, #13989, #15177, #12420, #18418, #1744, #6917, #5547, #840, #17404, #5361, #16036, #11321, #9936, #12698, #15653, #4070, #17223, #7109, #6821, #2224, #12889, #3978, #9845, #13071, #12788, #18701, #15932, #11603, #17315, #15841, #3879, #8216, #2405, #5643, #9759, #7010, #8485, #2596, #8387, #14463, #14360, #2498, #935, #5263, #18888, #5450, #11410, #17600, #19069, #1127, #12978, #9662, #8577, #14183, #11503, #10038, #1035, #14556, #18978, #17494, #748, #6731, #11218, #3792, #14271, #15753, #2315, #8298, #18786, #19364, #7301, #7600, #8964, #16326, #4272, #3083, #9064, #19269, #149, #16125, #14953, #14758 ),
 ( #15052, #10234, #5741, #5932, #1630, #11903, #16419, #17796, #14853, #17902, #1426, #55, #1331, #4474, #5838, #10525, #11802, #10425, #7204, #10128, #17995, #11701, #13568, #13268, #2694, #7401, #2984, #4369, #6134, #10330, #13177, #1527, #12095, #2894, #8868, #13372, #8670, #7496, #4177, #16218, #13472, #6040, #16520, #11997, #4568, #14653, #1222, #19170, #17694, #2790, #8767, #10819, #14058, #2109, #9546, #2007, #18093, #11016, #3190, #13964, #18489, #16818, #17015, #1917, #18391, #3573, #6334, #5057, #7903, #3287, #18295, #15538, #12487, #9259, #13867, #1817, #12394, #7699, #7796, #10917, #9454, #7998, #13665, #4775, #8093, #4863, #443, #15245, #3382, #13767, #6428, #246, #4961, #16916, #6230, #16623, #3480, #538, #1718, #6521, #9164, #15442, #10725, #633, #10622, #348, #9349, #15147, #6623, #4665, #12300, #15340, #12195, #18196, #16719, #12591, #11387, #5522, #729, #6708, #14339, #12679, #6988, #8556, #18583, #11111, #6894, #8370, #912, #14531, #15819, #17381, #12866, #819, #18681, #9916, #5246, #2385, #3954, #15733, #5149, #9642, #8463, #12954, #6804, #18953, #17107, #11482, #17470, #9824, #11199, #15627, #18867, #4046, #16016, #17202, #5429, #2294, #14439, #3671, #10012, #1103, #15911, #2575, #12768, #2197, #8192, #14161, #3767, #8278, #9736, #2475, #14248, #18764, #11298, #1013, #5337, #17294, #3860, #2962, #4345, #13248, #29, #2765, #4249, #11679, #7379, #7179, #17671, #10207, #14631, #4450, #17771 ),
 ( #1402, #5721, #2669, #16198, #9042, #8742, #1197, #14731, #7472, #10303, #16298, #8941, #4156, #16102, #1309, #13351, #5619, #17579, #2868, #10503, #13152, #19245, #8649, #19150, #19344, #7282, #5815, #13445, #10404, #11877, #11779, #10107, #17970, #5910, #17875, #8847, #14832, #16398, #19046, #14934, #1506, #6017, #11977, #4544, #16501, #15029, #3064, #7084, #13049, #11581, #3166, #3366, #18466, #16796, #13848, #15228, #12282, #9330, #18275, #16893, #12175, #15319, #16700, #7977, #3266, #1896, #4647, #7579, #15427, #9143, #5035, #18174, #13547, #4842, #7882, #1796, #10996, #4752, #10601, #424, #3557, #9236, #7778, #13744, #126, #328, #16997, #1695, #18374, #6408, #13943, #6311, #12373, #10798, #4941, #10898, #16600, #3460, #9434, #1991, #9526, #1605, #12465, #517, #6110, #6505, #12076, #18074, #15129, #7676, #13644, #228, #6212, #10705, #3744, #2455, #5312, #713, #15709, #8440, #9900, #6694, #11274, #18661, #9806, #5135, #5228, #8351, #6871, #5412, #11091, #2177, #15891, #2277, #17274, #12660, #8263, #11182, #3840, #17087, #15800, #2366, #3653, #14038, #14323, #11366, #18568, #17361, #608, #12842, #8167, #18843, #8075, #17180, #14231, #6604, #5498, #14416, #9717, #18930, #891, #799, #15607, #991, #6967, #6787, #11463, #12572, #12752, #18748, #12936, #3930, #17454, #4024, #15516, #14139, #2089, #9622, #17553, #7354, #1284, #5594, #1381, #10180, #4225, #16178, #4134, #4323, #8626, #11556, #14612, #11960, #7156 ),
 ( #7452, #5792, #2846, #2746, #7261, #11752, #13228, #5890, #1177, #17752, #5701, #16380, #11660, #10280, #13030, #15993, #4425, #10087, #13420, #13127, #2554, #19223, #16274, #8718, #6, #19126, #19028, #8828, #17952, #17650, #14707, #14813, #8536, #13323, #5994, #16080, #19323, #11850, #2943, #17853, #10387, #8919, #14910, #1484, #2644, #9987, #14510, #1081, #7060, #7953, #15400, #7856, #4524, #16870, #9018, #402, #4917, #3242, #3433, #7757, #4823, #9406, #12150, #10876, #13721, #9119, #4724, #1970, #18346, #15108, #298, #7655, #18252, #13530, #13621, #16774, #15298, #13825, #107, #10581, #13916, #10681, #6286, #1678, #16679, #206, #12256, #6090, #10771, #3344, #12054, #3044, #9312, #6385, #7553, #12348, #15004, #493, #4626, #6194, #18052, #1870, #18149, #16574, #9215, #6479, #12446, #1581, #15206, #10482, #1774, #16475, #3141, #14116, #15587, #3627, #18723, #18546, #9597, #2155, #6578, #16038, #9691, #14014, #10041, #18634, #12637, #5202, #12545, #12728, #17066, #586, #8143, #1226, #690, #5113, #6674, #19072, #15684, #2254, #14559, #15492, #8052, #11158, #5287, #16974, #9504, #8242, #2699, #11066, #17156, #3718, #14209, #11246, #775, #6759, #5646, #2598, #4074, #17249, #2061, #10131, #8579, #1132, #7111, #13074, #11606, #10971, #17602, #4179, #16127, #8673, #14655, #18443, #7207, #5011, #3534, #7303, #14955, #13270, #7604, #9167, #13180, #11703, #7499, #8968, #1529, #15151, #16421, #17997, #13476, #1428, #19271 ),
 ( #10237, #9067, #13570, #7405, #151, #17696, #6136, #12099, #10428, #1333, #16222, #59, #18095, #16626, #5842, #2986, #16329, #15055, #19172, #4667, #1721, #16522, #10624, #13374, #4276, #3192, #10529, #2793, #14855, #5743, #8770, #1633, #14761, #11804, #17799, #6042, #4374, #11999, #4570, #19366, #4476, #3085, #10333, #2896, #8870, #5936, #11908, #17904, #9351, #8000, #10727, #13668, #2111, #15249, #5152, #4865, #248, #4963, #2011, #7905, #11113, #18297, #16722, #15444, #9644, #15343, #13870, #1922, #6232, #445, #3674, #7798, #5060, #6525, #636, #6430, #12490, #3384, #13966, #18396, #3291, #10919, #12396, #16919, #15630, #17109, #18585, #11018, #7701, #6626, #12198, #3577, #8095, #3483, #12593, #9458, #540, #18200, #18492, #14062, #17020, #12302, #9549, #4777, #9261, #10823, #15540, #16821, #1819, #13770, #350, #6337, #12961, #11487, #17204, #8281, #16020, #2387, #3957, #6806, #14343, #12771, #17384, #11201, #11390, #2478, #3770, #731, #15916, #17475, #5249, #4050, #6711, #18957, #14251, #5526, #14163, #18766, #8374, #12681, #11586, #14537, #5339, #5623, #6992, #915, #2296, #1108, #7088, #17299, #17584, #18683, #10017, #11301, #6898, #2579, #9919, #9741, #3862, #8559, #18870, #12871, #13053, #9827, #15821, #5434, #8467, #822, #14443, #1018, #15735, #19051, #4160, #10111, #2202, #8195, #10309, #2874, #4253, #10409, #14736, #11683, #1315, #18080, #13253, #10211, #5820, #16506, #13356, #19349, #11982, #13157, #5725 ) ),
 .UNSPECIFIED., .T., .F., .F. ) 
 B_SPLINE_SURFACE_WITH_KNOTS ( ( 4, 3, 4 ),
 ( 3, 2, 2, 2, 2, 2, 2, 2, 2, 2, 2, 2, 2, 2, 2, 2, 2, 2, 2, 2, 2, 2, 2, 2, 2, 2, 2, 2, 2, 2, 2, 2, 2, 2, 2, 2, 2, 2, 2, 2, 2, 2, 2, 2, 2, 2, 2, 2, 2, 2, 2, 2, 2, 2, 2, 2, 2, 2, 2, 2, 2, 2, 2, 2, 2, 2, 2, 2, 2, 2, 2, 2, 2, 2, 2, 2, 2, 2, 2, 2, 2, 2, 2, 2, 2, 2, 2, 2, 2, 2, 2, 2, 2, 2, 2, 2, 3 ),
 ( 0.000000000000000000, 0.5000000000000000000, 1.000000000000000000 ),
 ( 0.000000000000000000, 0.01041666666666666609, 0.02083333333333333218, 0.03125000000000000000, 0.04166666666666666435, 0.05208333333333333565, 0.06250000000000000000, 0.07291666666666667129, 0.08333333333333332871, 0.09375000000000000000, 0.1041666666666666713, 0.1145833333333333287, 0.1250000000000000000, 0.1354166666666666574, 0.1458333333333333426, 0.1562500000000000000, 0.1666666666666666574, 0.1770833333333333426, 0.1875000000000000000, 0.1979166666666666574, 0.2083333333333333426, 0.2187500000000000000, 0.2291666666666666574, 0.2395833333333333426, 0.2500000000000000000, 0.2604166666666666852, 0.2708333333333333148, 0.2812500000000000000, 0.2916666666666666852, 0.3020833333333333148, 0.3125000000000000000, 0.3229166666666666852, 0.3333333333333333148, 0.3437500000000000000, 0.3541666666666666852, 0.3645833333333333148, 0.3750000000000000000, 0.3854166666666666852, 0.3958333333333333148, 0.4062500000000000000, 0.4166666666666666852, 0.4270833333333333148, 0.4375000000000000000, 0.4479166666666666852, 0.4583333333333333148, 0.4687500000000000000, 0.4791666666666666852, 0.4895833333333333148, 0.5000000000000000000, 0.5104166666666666297, 0.5208333333333333703, 0.5312500000000000000, 0.5416666666666666297, 0.5520833333333333703, 0.5625000000000000000, 0.5729166666666666297, 0.5833333333333333703, 0.5937500000000000000, 0.6041666666666666297, 0.6145833333333333703, 0.6250000000000000000, 0.6354166666666666297, 0.6458333333333333703, 0.6562500000000000000, 0.6666666666666666297, 0.6770833333333333703, 0.6875000000000000000, 0.6979166666666666297, 0.7083333333333333703, 0.7187500000000000000, 0.7291666666666666297, 0.7395833333333333703, 0.7500000000000000000, 0.7604166666666666297, 0.7708333333333333703, 0.7812500000000000000, 0.7916666666666666297, 0.8020833333333333703, 0.8125000000000000000, 0.8229166666666666297, 0.8333333333333333703, 0.8437500000000000000, 0.8541666666666666297, 0.8645833333333333703, 0.8750000000000000000, 0.8854166666666666297, 0.8958333333333333703, 0.9062500000000000000, 0.9166666666666666297, 0.9270833333333333703, 0.9375000000000000000, 0.9479166666666666297, 0.9583333333333333703, 0.9687500000000000000, 0.9791666666666666297, 0.9895833333333333703, 1.000000000000000000 ),
 .UNSPECIFIED. ) 
 GEOMETRIC_REPRESENTATION_ITEM ( )  RATIONAL_B_SPLINE_SURFACE ( (
 ( 1.000000000000000000, 0.9659258262890683122, 1.000000000000000000, 0.9659258262890683122, 1.000000000000000000, 0.9659258262890683122, 1.000000000000000000, 0.9659258262890683122, 1.000000000000000000, 0.9659258262890683122, 1.000000000000000000, 0.9659258262890683122, 1.000000000000000000, 0.9659258262890683122, 1.000000000000000000, 0.9659258262890683122, 1.000000000000000000, 0.9659258262890683122, 1.000000000000000000, 0.9659258262890683122, 1.000000000000000000, 0.9659258262890683122, 1.000000000000000000, 0.9659258262890683122, 1.000000000000000000, 0.9659258262890683122, 1.000000000000000000, 0.9659258262890683122, 1.000000000000000000, 0.9659258262890683122, 1.000000000000000000, 0.9659258262890683122, 1.000000000000000000, 0.9659258262890683122, 1.000000000000000000, 0.9659258262890683122, 1.000000000000000000, 0.9659258262890683122, 1.000000000000000000, 0.9659258262890683122, 1.000000000000000000, 0.9659258262890683122, 1.000000000000000000, 0.9659258262890683122, 1.000000000000000000, 0.9659258262890683122, 1.000000000000000000, 0.9659258262890683122, 1.000000000000000000, 0.9659258262890683122, 1.000000000000000000, 0.9659258262890683122, 1.000000000000000000, 0.9659258262890683122, 1.000000000000000000, 0.9659258262890683122, 1.000000000000000000, 0.9659258262890683122, 1.000000000000000000, 0.9659258262890683122, 1.000000000000000000, 0.9659258262890683122, 1.000000000000000000, 0.9659258262890683122, 1.000000000000000000, 0.9659258262890683122, 1.000000000000000000, 0.9659258262890683122, 1.000000000000000000, 0.9659258262890683122, 1.000000000000000000, 0.9659258262890683122, 1.000000000000000000, 0.9659258262890683122, 1.000000000000000000, 0.9659258262890683122, 1.000000000000000000, 0.9659258262890683122, 1.000000000000000000, 0.9659258262890683122, 1.000000000000000000, 0.9659258262890683122, 1.000000000000000000, 0.9659258262890683122, 1.000000000000000000, 0.9659258262890683122, 1.000000000000000000, 0.9659258262890683122, 1.000000000000000000, 0.9659258262890683122, 1.000000000000000000, 0.9659258262890683122, 1.000000000000000000, 0.9659258262890683122, 1.000000000000000000, 0.9659258262890683122, 1.000000000000000000, 0.9659258262890683122, 1.000000000000000000, 0.9659258262890683122, 1.000000000000000000, 0.9659258262890683122, 1.000000000000000000, 0.9659258262890683122, 1.000000000000000000, 0.9659258262890683122, 1.000000000000000000, 0.9659258262890683122, 1.000000000000000000, 0.9659258262890683122, 1.000000000000000000, 0.9659258262890683122, 1.000000000000000000, 0.9659258262890683122, 1.000000000000000000, 0.9659258262890683122, 1.000000000000000000, 0.9659258262890683122, 1.000000000000000000, 0.9659258262890683122, 1.000000000000000000, 0.9659258262890683122, 1.000000000000000000, 0.9659258262890683122, 1.000000000000000000, 0.9659258262890683122, 1.000000000000000000, 0.9659258262890683122, 1.000000000000000000, 0.9659258262890683122, 1.000000000000000000, 0.9659258262890683122, 1.000000000000000000, 0.9659258262890683122, 1.000000000000000000, 0.9659258262890683122, 1.000000000000000000, 0.9659258262890683122, 1.000000000000000000, 0.9659258262890683122, 1.000000000000000000, 0.9659258262890683122, 1.000000000000000000, 0.9659258262890683122, 1.000000000000000000, 0.9659258262890683122, 1.000000000000000000, 0.9659258262890683122, 1.000000000000000000, 0.9659258262890683122, 1.000000000000000000, 0.9659258262890683122, 1.000000000000000000, 0.9659258262890683122, 1.000000000000000000, 0.9659258262890683122, 1.000000000000000000, 0.9659258262890683122, 1.000000000000000000, 0.9659258262890683122, 1.000000000000000000, 0.9659258262890683122, 1.000000000000000000, 0.9659258262890683122, 1.000000000000000000, 0.9659258262890683122, 1.000000000000000000, 0.9659258262890683122, 1.000000000000000000, 0.9659258262890683122, 1.000000000000000000, 0.9659258262890683122, 1.000000000000000000, 0.9659258262890683122, 1.000000000000000000, 0.9659258262890683122, 1.000000000000000000, 0.9659258262890683122, 1.000000000000000000, 0.9659258262890683122, 1.000000000000000000, 0.9659258262890683122, 1.000000000000000000, 0.9659258262890683122, 1.000000000000000000, 0.9659258262890683122, 1.000000000000000000, 0.9659258262890683122, 1.000000000000000000, 0.9659258262890683122, 1.000000000000000000, 0.9659258262890683122, 1.000000000000000000),
 ( 0.3333333333333333703, 0.3219752754296894559, 0.3333333333333333703, 0.3219752754296894559, 0.3333333333333333703, 0.3219752754296894559, 0.3333333333333333703, 0.3219752754296894559, 0.3333333333333333703, 0.3219752754296894559, 0.3333333333333333703, 0.3219752754296894559, 0.3333333333333333703, 0.3219752754296894559, 0.3333333333333333703, 0.3219752754296894559, 0.3333333333333333703, 0.3219752754296894559, 0.3333333333333333703, 0.3219752754296894559, 0.3333333333333333703, 0.3219752754296894559, 0.3333333333333333703, 0.3219752754296894559, 0.3333333333333333703, 0.3219752754296894559, 0.3333333333333333703, 0.3219752754296894559, 0.3333333333333333703, 0.3219752754296894559, 0.3333333333333333703, 0.3219752754296894559, 0.3333333333333333703, 0.3219752754296894559, 0.3333333333333333703, 0.3219752754296894559, 0.3333333333333333703, 0.3219752754296894559, 0.3333333333333333703, 0.3219752754296894559, 0.3333333333333333703, 0.3219752754296894559, 0.3333333333333333703, 0.3219752754296894559, 0.3333333333333333703, 0.3219752754296894559, 0.3333333333333333703, 0.3219752754296894559, 0.3333333333333333703, 0.3219752754296894559, 0.3333333333333333703, 0.3219752754296894559, 0.3333333333333333703, 0.3219752754296894559, 0.3333333333333333703, 0.3219752754296894559, 0.3333333333333333703, 0.3219752754296894559, 0.3333333333333333703, 0.3219752754296894559, 0.3333333333333333703, 0.3219752754296894559, 0.3333333333333333703, 0.3219752754296894559, 0.3333333333333333703, 0.3219752754296894559, 0.3333333333333333703, 0.3219752754296894559, 0.3333333333333333703, 0.3219752754296894559, 0.3333333333333333703, 0.3219752754296894559, 0.3333333333333333703, 0.3219752754296894559, 0.3333333333333333703, 0.3219752754296894559, 0.3333333333333333703, 0.3219752754296894559, 0.3333333333333333703, 0.3219752754296894559, 0.3333333333333333703, 0.3219752754296894559, 0.3333333333333333703, 0.3219752754296894559, 0.3333333333333333703, 0.3219752754296894559, 0.3333333333333333703, 0.3219752754296894559, 0.3333333333333333703, 0.3219752754296894559, 0.3333333333333333703, 0.3219752754296894559, 0.3333333333333333703, 0.3219752754296894559, 0.3333333333333333703, 0.3219752754296894559, 0.3333333333333333703, 0.3219752754296894559, 0.3333333333333333703, 0.3219752754296894559, 0.3333333333333333703, 0.3219752754296894559, 0.3333333333333333703, 0.3219752754296894559, 0.3333333333333333703, 0.3219752754296894559, 0.3333333333333333703, 0.3219752754296894559, 0.3333333333333333703, 0.3219752754296894559, 0.3333333333333333703, 0.3219752754296894559, 0.3333333333333333703, 0.3219752754296894559, 0.3333333333333333703, 0.3219752754296894559, 0.3333333333333333703, 0.3219752754296894559, 0.3333333333333333703, 0.3219752754296894559, 0.3333333333333333703, 0.3219752754296894559, 0.3333333333333333703, 0.3219752754296894559, 0.3333333333333333703, 0.3219752754296894559, 0.3333333333333333703, 0.3219752754296894559, 0.3333333333333333703, 0.3219752754296894559, 0.3333333333333333703, 0.3219752754296894559, 0.3333333333333333703, 0.3219752754296894559, 0.3333333333333333703, 0.3219752754296894559, 0.3333333333333333703, 0.3219752754296894559, 0.3333333333333333703, 0.3219752754296894559, 0.3333333333333333703, 0.3219752754296894559, 0.3333333333333333703, 0.3219752754296894559, 0.3333333333333333703, 0.3219752754296894559, 0.3333333333333333703, 0.3219752754296894559, 0.3333333333333333703, 0.3219752754296894559, 0.3333333333333333703, 0.3219752754296894559, 0.3333333333333333703, 0.3219752754296894559, 0.3333333333333333703, 0.3219752754296894559, 0.3333333333333333703, 0.3219752754296894559, 0.3333333333333333703, 0.3219752754296894559, 0.3333333333333333703, 0.3219752754296894559, 0.3333333333333333703, 0.3219752754296894559, 0.3333333333333333703, 0.3219752754296894559, 0.3333333333333333703, 0.3219752754296894559, 0.3333333333333333703, 0.3219752754296894559, 0.3333333333333333703, 0.3219752754296894559, 0.3333333333333333703, 0.3219752754296894559, 0.3333333333333333703, 0.3219752754296894559, 0.3333333333333333703, 0.3219752754296894559, 0.3333333333333333703, 0.3219752754296894559, 0.3333333333333333703, 0.3219752754296894559, 0.3333333333333333703, 0.3219752754296894559, 0.3333333333333333703, 0.3219752754296894559, 0.3333333333333333703, 0.3219752754296894559, 0.3333333333333333703, 0.3219752754296894559, 0.3333333333333333703, 0.3219752754296894559, 0.3333333333333333703),
 ( 0.3333333333333333703, 0.3219752754296894559, 0.3333333333333333703, 0.3219752754296894559, 0.3333333333333333703, 0.3219752754296894559, 0.3333333333333333703, 0.3219752754296894559, 0.3333333333333333703, 0.3219752754296894559, 0.3333333333333333703, 0.3219752754296894559, 0.3333333333333333703, 0.3219752754296894559, 0.3333333333333333703, 0.3219752754296894559, 0.3333333333333333703, 0.3219752754296894559, 0.3333333333333333703, 0.3219752754296894559, 0.3333333333333333703, 0.3219752754296894559, 0.3333333333333333703, 0.3219752754296894559, 0.3333333333333333703, 0.3219752754296894559, 0.3333333333333333703, 0.3219752754296894559, 0.3333333333333333703, 0.3219752754296894559, 0.3333333333333333703, 0.3219752754296894559, 0.3333333333333333703, 0.3219752754296894559, 0.3333333333333333703, 0.3219752754296894559, 0.3333333333333333703, 0.3219752754296894559, 0.3333333333333333703, 0.3219752754296894559, 0.3333333333333333703, 0.3219752754296894559, 0.3333333333333333703, 0.3219752754296894559, 0.3333333333333333703, 0.3219752754296894559, 0.3333333333333333703, 0.3219752754296894559, 0.3333333333333333703, 0.3219752754296894559, 0.3333333333333333703, 0.3219752754296894559, 0.3333333333333333703, 0.3219752754296894559, 0.3333333333333333703, 0.3219752754296894559, 0.3333333333333333703, 0.3219752754296894559, 0.3333333333333333703, 0.3219752754296894559, 0.3333333333333333703, 0.3219752754296894559, 0.3333333333333333703, 0.3219752754296894559, 0.3333333333333333703, 0.3219752754296894559, 0.3333333333333333703, 0.3219752754296894559, 0.3333333333333333703, 0.3219752754296894559, 0.3333333333333333703, 0.3219752754296894559, 0.3333333333333333703, 0.3219752754296894559, 0.3333333333333333703, 0.3219752754296894559, 0.3333333333333333703, 0.3219752754296894559, 0.3333333333333333703, 0.3219752754296894559, 0.3333333333333333703, 0.3219752754296894559, 0.3333333333333333703, 0.3219752754296894559, 0.3333333333333333703, 0.3219752754296894559, 0.3333333333333333703, 0.3219752754296894559, 0.3333333333333333703, 0.3219752754296894559, 0.3333333333333333703, 0.3219752754296894559, 0.3333333333333333703, 0.3219752754296894559, 0.3333333333333333703, 0.3219752754296894559, 0.3333333333333333703, 0.3219752754296894559, 0.3333333333333333703, 0.3219752754296894559, 0.3333333333333333703, 0.3219752754296894559, 0.3333333333333333703, 0.3219752754296894559, 0.3333333333333333703, 0.3219752754296894559, 0.3333333333333333703, 0.3219752754296894559, 0.3333333333333333703, 0.3219752754296894559, 0.3333333333333333703, 0.3219752754296894559, 0.3333333333333333703, 0.3219752754296894559, 0.3333333333333333703, 0.3219752754296894559, 0.3333333333333333703, 0.3219752754296894559, 0.3333333333333333703, 0.3219752754296894559, 0.3333333333333333703, 0.3219752754296894559, 0.3333333333333333703, 0.3219752754296894559, 0.3333333333333333703, 0.3219752754296894559, 0.3333333333333333703, 0.3219752754296894559, 0.3333333333333333703, 0.3219752754296894559, 0.3333333333333333703, 0.3219752754296894559, 0.3333333333333333703, 0.3219752754296894559, 0.3333333333333333703, 0.3219752754296894559, 0.3333333333333333703, 0.3219752754296894559, 0.3333333333333333703, 0.3219752754296894559, 0.3333333333333333703, 0.3219752754296894559, 0.3333333333333333703, 0.3219752754296894559, 0.3333333333333333703, 0.3219752754296894559, 0.3333333333333333703, 0.3219752754296894559, 0.3333333333333333703, 0.3219752754296894559, 0.3333333333333333703, 0.3219752754296894559, 0.3333333333333333703, 0.3219752754296894559, 0.3333333333333333703, 0.3219752754296894559, 0.3333333333333333703, 0.3219752754296894559, 0.3333333333333333703, 0.3219752754296894559, 0.3333333333333333703, 0.3219752754296894559, 0.3333333333333333703, 0.3219752754296894559, 0.3333333333333333703, 0.3219752754296894559, 0.3333333333333333703, 0.3219752754296894559, 0.3333333333333333703, 0.3219752754296894559, 0.3333333333333333703, 0.3219752754296894559, 0.3333333333333333703, 0.3219752754296894559, 0.3333333333333333703, 0.3219752754296894559, 0.3333333333333333703, 0.3219752754296894559, 0.3333333333333333703, 0.3219752754296894559, 0.3333333333333333703, 0.3219752754296894559, 0.3333333333333333703, 0.3219752754296894559, 0.3333333333333333703, 0.3219752754296894559, 0.3333333333333333703, 0.3219752754296894559, 0.3333333333333333703, 0.3219752754296894559, 0.3333333333333333703, 0.3219752754296894559, 0.3333333333333333703),
 ( 1.000000000000000000, 0.9659258262890683122, 1.000000000000000000, 0.9659258262890683122, 1.000000000000000000, 0.9659258262890683122, 1.000000000000000000, 0.9659258262890683122, 1.000000000000000000, 0.9659258262890683122, 1.000000000000000000, 0.9659258262890683122, 1.000000000000000000, 0.9659258262890683122, 1.000000000000000000, 0.9659258262890683122, 1.000000000000000000, 0.9659258262890683122, 1.000000000000000000, 0.9659258262890683122, 1.000000000000000000, 0.9659258262890683122, 1.000000000000000000, 0.9659258262890683122, 1.000000000000000000, 0.9659258262890683122, 1.000000000000000000, 0.9659258262890683122, 1.000000000000000000, 0.9659258262890683122, 1.000000000000000000, 0.9659258262890683122, 1.000000000000000000, 0.9659258262890683122, 1.000000000000000000, 0.9659258262890683122, 1.000000000000000000, 0.9659258262890683122, 1.000000000000000000, 0.9659258262890683122, 1.000000000000000000, 0.9659258262890683122, 1.000000000000000000, 0.9659258262890683122, 1.000000000000000000, 0.9659258262890683122, 1.000000000000000000, 0.9659258262890683122, 1.000000000000000000, 0.9659258262890683122, 1.000000000000000000, 0.9659258262890683122, 1.000000000000000000, 0.9659258262890683122, 1.000000000000000000, 0.9659258262890683122, 1.000000000000000000, 0.9659258262890683122, 1.000000000000000000, 0.9659258262890683122, 1.000000000000000000, 0.9659258262890683122, 1.000000000000000000, 0.9659258262890683122, 1.000000000000000000, 0.9659258262890683122, 1.000000000000000000, 0.9659258262890683122, 1.000000000000000000, 0.9659258262890683122, 1.000000000000000000, 0.9659258262890683122, 1.000000000000000000, 0.9659258262890683122, 1.000000000000000000, 0.9659258262890683122, 1.000000000000000000, 0.9659258262890683122, 1.000000000000000000, 0.9659258262890683122, 1.000000000000000000, 0.9659258262890683122, 1.000000000000000000, 0.9659258262890683122, 1.000000000000000000, 0.9659258262890683122, 1.000000000000000000, 0.9659258262890683122, 1.000000000000000000, 0.9659258262890683122, 1.000000000000000000, 0.9659258262890683122, 1.000000000000000000, 0.9659258262890683122, 1.000000000000000000, 0.9659258262890683122, 1.000000000000000000, 0.9659258262890683122, 1.000000000000000000, 0.9659258262890683122, 1.000000000000000000, 0.9659258262890683122, 1.000000000000000000, 0.9659258262890683122, 1.000000000000000000, 0.9659258262890683122, 1.000000000000000000, 0.9659258262890683122, 1.000000000000000000, 0.9659258262890683122, 1.000000000000000000, 0.9659258262890683122, 1.000000000000000000, 0.9659258262890683122, 1.000000000000000000, 0.9659258262890683122, 1.000000000000000000, 0.9659258262890683122, 1.000000000000000000, 0.9659258262890683122, 1.000000000000000000, 0.9659258262890683122, 1.000000000000000000, 0.9659258262890683122, 1.000000000000000000, 0.9659258262890683122, 1.000000000000000000, 0.9659258262890683122, 1.000000000000000000, 0.9659258262890683122, 1.000000000000000000, 0.9659258262890683122, 1.000000000000000000, 0.9659258262890683122, 1.000000000000000000, 0.9659258262890683122, 1.000000000000000000, 0.9659258262890683122, 1.000000000000000000, 0.9659258262890683122, 1.000000000000000000, 0.9659258262890683122, 1.000000000000000000, 0.9659258262890683122, 1.000000000000000000, 0.9659258262890683122, 1.000000000000000000, 0.9659258262890683122, 1.000000000000000000, 0.9659258262890683122, 1.000000000000000000, 0.9659258262890683122, 1.000000000000000000, 0.9659258262890683122, 1.000000000000000000, 0.9659258262890683122, 1.000000000000000000, 0.9659258262890683122, 1.000000000000000000, 0.9659258262890683122, 1.000000000000000000, 0.9659258262890683122, 1.000000000000000000, 0.9659258262890683122, 1.000000000000000000, 0.9659258262890683122, 1.000000000000000000, 0.9659258262890683122, 1.000000000000000000, 0.9659258262890683122, 1.000000000000000000, 0.9659258262890683122, 1.000000000000000000, 0.9659258262890683122, 1.000000000000000000, 0.9659258262890683122, 1.000000000000000000, 0.9659258262890683122, 1.000000000000000000, 0.9659258262890683122, 1.000000000000000000, 0.9659258262890683122, 1.000000000000000000, 0.9659258262890683122, 1.000000000000000000, 0.9659258262890683122, 1.000000000000000000, 0.9659258262890683122, 1.000000000000000000, 0.9659258262890683122, 1.000000000000000000, 0.9659258262890683122, 1.000000000000000000),
 ( 0.3333333333333333703, 0.3219752754296894559, 0.3333333333333333703, 0.3219752754296894559, 0.3333333333333333703, 0.3219752754296894559, 0.3333333333333333703, 0.3219752754296894559, 0.3333333333333333703, 0.3219752754296894559, 0.3333333333333333703, 0.3219752754296894559, 0.3333333333333333703, 0.3219752754296894559, 0.3333333333333333703, 0.3219752754296894559, 0.3333333333333333703, 0.3219752754296894559, 0.3333333333333333703, 0.3219752754296894559, 0.3333333333333333703, 0.3219752754296894559, 0.3333333333333333703, 0.3219752754296894559, 0.3333333333333333703, 0.3219752754296894559, 0.3333333333333333703, 0.3219752754296894559, 0.3333333333333333703, 0.3219752754296894559, 0.3333333333333333703, 0.3219752754296894559, 0.3333333333333333703, 0.3219752754296894559, 0.3333333333333333703, 0.3219752754296894559, 0.3333333333333333703, 0.3219752754296894559, 0.3333333333333333703, 0.3219752754296894559, 0.3333333333333333703, 0.3219752754296894559, 0.3333333333333333703, 0.3219752754296894559, 0.3333333333333333703, 0.3219752754296894559, 0.3333333333333333703, 0.3219752754296894559, 0.3333333333333333703, 0.3219752754296894559, 0.3333333333333333703, 0.3219752754296894559, 0.3333333333333333703, 0.3219752754296894559, 0.3333333333333333703, 0.3219752754296894559, 0.3333333333333333703, 0.3219752754296894559, 0.3333333333333333703, 0.3219752754296894559, 0.3333333333333333703, 0.3219752754296894559, 0.3333333333333333703, 0.3219752754296894559, 0.3333333333333333703, 0.3219752754296894559, 0.3333333333333333703, 0.3219752754296894559, 0.3333333333333333703, 0.3219752754296894559, 0.3333333333333333703, 0.3219752754296894559, 0.3333333333333333703, 0.3219752754296894559, 0.3333333333333333703, 0.3219752754296894559, 0.3333333333333333703, 0.3219752754296894559, 0.3333333333333333703, 0.3219752754296894559, 0.3333333333333333703, 0.3219752754296894559, 0.3333333333333333703, 0.3219752754296894559, 0.3333333333333333703, 0.3219752754296894559, 0.3333333333333333703, 0.3219752754296894559, 0.3333333333333333703, 0.3219752754296894559, 0.3333333333333333703, 0.3219752754296894559, 0.3333333333333333703, 0.3219752754296894559, 0.3333333333333333703, 0.3219752754296894559, 0.3333333333333333703, 0.3219752754296894559, 0.3333333333333333703, 0.3219752754296894559, 0.3333333333333333703, 0.3219752754296894559, 0.3333333333333333703, 0.3219752754296894559, 0.3333333333333333703, 0.3219752754296894559, 0.3333333333333333703, 0.3219752754296894559, 0.3333333333333333703, 0.3219752754296894559, 0.3333333333333333703, 0.3219752754296894559, 0.3333333333333333703, 0.3219752754296894559, 0.3333333333333333703, 0.3219752754296894559, 0.3333333333333333703, 0.3219752754296894559, 0.3333333333333333703, 0.3219752754296894559, 0.3333333333333333703, 0.3219752754296894559, 0.3333333333333333703, 0.3219752754296894559, 0.3333333333333333703, 0.3219752754296894559, 0.3333333333333333703, 0.3219752754296894559, 0.3333333333333333703, 0.3219752754296894559, 0.3333333333333333703, 0.3219752754296894559, 0.3333333333333333703, 0.3219752754296894559, 0.3333333333333333703, 0.3219752754296894559, 0.3333333333333333703, 0.3219752754296894559, 0.3333333333333333703, 0.3219752754296894559, 0.3333333333333333703, 0.3219752754296894559, 0.3333333333333333703, 0.3219752754296894559, 0.3333333333333333703, 0.3219752754296894559, 0.3333333333333333703, 0.3219752754296894559, 0.3333333333333333703, 0.3219752754296894559, 0.3333333333333333703, 0.3219752754296894559, 0.3333333333333333703, 0.3219752754296894559, 0.3333333333333333703, 0.3219752754296894559, 0.3333333333333333703, 0.3219752754296894559, 0.3333333333333333703, 0.3219752754296894559, 0.3333333333333333703, 0.3219752754296894559, 0.3333333333333333703, 0.3219752754296894559, 0.3333333333333333703, 0.3219752754296894559, 0.3333333333333333703, 0.3219752754296894559, 0.3333333333333333703, 0.3219752754296894559, 0.3333333333333333703, 0.3219752754296894559, 0.3333333333333333703, 0.3219752754296894559, 0.3333333333333333703, 0.3219752754296894559, 0.3333333333333333703, 0.3219752754296894559, 0.3333333333333333703, 0.3219752754296894559, 0.3333333333333333703, 0.3219752754296894559, 0.3333333333333333703, 0.3219752754296894559, 0.3333333333333333703, 0.3219752754296894559, 0.3333333333333333703, 0.3219752754296894559, 0.3333333333333333703, 0.3219752754296894559, 0.3333333333333333703, 0.3219752754296894559, 0.3333333333333333703),
 ( 0.3333333333333333703, 0.3219752754296894559, 0.3333333333333333703, 0.3219752754296894559, 0.3333333333333333703, 0.3219752754296894559, 0.3333333333333333703, 0.3219752754296894559, 0.3333333333333333703, 0.3219752754296894559, 0.3333333333333333703, 0.3219752754296894559, 0.3333333333333333703, 0.3219752754296894559, 0.3333333333333333703, 0.3219752754296894559, 0.3333333333333333703, 0.3219752754296894559, 0.3333333333333333703, 0.3219752754296894559, 0.3333333333333333703, 0.3219752754296894559, 0.3333333333333333703, 0.3219752754296894559, 0.3333333333333333703, 0.3219752754296894559, 0.3333333333333333703, 0.3219752754296894559, 0.3333333333333333703, 0.3219752754296894559, 0.3333333333333333703, 0.3219752754296894559, 0.3333333333333333703, 0.3219752754296894559, 0.3333333333333333703, 0.3219752754296894559, 0.3333333333333333703, 0.3219752754296894559, 0.3333333333333333703, 0.3219752754296894559, 0.3333333333333333703, 0.3219752754296894559, 0.3333333333333333703, 0.3219752754296894559, 0.3333333333333333703, 0.3219752754296894559, 0.3333333333333333703, 0.3219752754296894559, 0.3333333333333333703, 0.3219752754296894559, 0.3333333333333333703, 0.3219752754296894559, 0.3333333333333333703, 0.3219752754296894559, 0.3333333333333333703, 0.3219752754296894559, 0.3333333333333333703, 0.3219752754296894559, 0.3333333333333333703, 0.3219752754296894559, 0.3333333333333333703, 0.3219752754296894559, 0.3333333333333333703, 0.3219752754296894559, 0.3333333333333333703, 0.3219752754296894559, 0.3333333333333333703, 0.3219752754296894559, 0.3333333333333333703, 0.3219752754296894559, 0.3333333333333333703, 0.3219752754296894559, 0.3333333333333333703, 0.3219752754296894559, 0.3333333333333333703, 0.3219752754296894559, 0.3333333333333333703, 0.3219752754296894559, 0.3333333333333333703, 0.3219752754296894559, 0.3333333333333333703, 0.3219752754296894559, 0.3333333333333333703, 0.3219752754296894559, 0.3333333333333333703, 0.3219752754296894559, 0.3333333333333333703, 0.3219752754296894559, 0.3333333333333333703, 0.3219752754296894559, 0.3333333333333333703, 0.3219752754296894559, 0.3333333333333333703, 0.3219752754296894559, 0.3333333333333333703, 0.3219752754296894559, 0.3333333333333333703, 0.3219752754296894559, 0.3333333333333333703, 0.3219752754296894559, 0.3333333333333333703, 0.3219752754296894559, 0.3333333333333333703, 0.3219752754296894559, 0.3333333333333333703, 0.3219752754296894559, 0.3333333333333333703, 0.3219752754296894559, 0.3333333333333333703, 0.3219752754296894559, 0.3333333333333333703, 0.3219752754296894559, 0.3333333333333333703, 0.3219752754296894559, 0.3333333333333333703, 0.3219752754296894559, 0.3333333333333333703, 0.3219752754296894559, 0.3333333333333333703, 0.3219752754296894559, 0.3333333333333333703, 0.3219752754296894559, 0.3333333333333333703, 0.3219752754296894559, 0.3333333333333333703, 0.3219752754296894559, 0.3333333333333333703, 0.3219752754296894559, 0.3333333333333333703, 0.3219752754296894559, 0.3333333333333333703, 0.3219752754296894559, 0.3333333333333333703, 0.3219752754296894559, 0.3333333333333333703, 0.3219752754296894559, 0.3333333333333333703, 0.3219752754296894559, 0.3333333333333333703, 0.3219752754296894559, 0.3333333333333333703, 0.3219752754296894559, 0.3333333333333333703, 0.3219752754296894559, 0.3333333333333333703, 0.3219752754296894559, 0.3333333333333333703, 0.3219752754296894559, 0.3333333333333333703, 0.3219752754296894559, 0.3333333333333333703, 0.3219752754296894559, 0.3333333333333333703, 0.3219752754296894559, 0.3333333333333333703, 0.3219752754296894559, 0.3333333333333333703, 0.3219752754296894559, 0.3333333333333333703, 0.3219752754296894559, 0.3333333333333333703, 0.3219752754296894559, 0.3333333333333333703, 0.3219752754296894559, 0.3333333333333333703, 0.3219752754296894559, 0.3333333333333333703, 0.3219752754296894559, 0.3333333333333333703, 0.3219752754296894559, 0.3333333333333333703, 0.3219752754296894559, 0.3333333333333333703, 0.3219752754296894559, 0.3333333333333333703, 0.3219752754296894559, 0.3333333333333333703, 0.3219752754296894559, 0.3333333333333333703, 0.3219752754296894559, 0.3333333333333333703, 0.3219752754296894559, 0.3333333333333333703, 0.3219752754296894559, 0.3333333333333333703, 0.3219752754296894559, 0.3333333333333333703, 0.3219752754296894559, 0.3333333333333333703, 0.3219752754296894559, 0.3333333333333333703, 0.3219752754296894559, 0.3333333333333333703),
 ( 1.000000000000000000, 0.9659258262890683122, 1.000000000000000000, 0.9659258262890683122, 1.000000000000000000, 0.9659258262890683122, 1.000000000000000000, 0.9659258262890683122, 1.000000000000000000, 0.9659258262890683122, 1.000000000000000000, 0.9659258262890683122, 1.000000000000000000, 0.9659258262890683122, 1.000000000000000000, 0.9659258262890683122, 1.000000000000000000, 0.9659258262890683122, 1.000000000000000000, 0.9659258262890683122, 1.000000000000000000, 0.9659258262890683122, 1.000000000000000000, 0.9659258262890683122, 1.000000000000000000, 0.9659258262890683122, 1.000000000000000000, 0.9659258262890683122, 1.000000000000000000, 0.9659258262890683122, 1.000000000000000000, 0.9659258262890683122, 1.000000000000000000, 0.9659258262890683122, 1.000000000000000000, 0.9659258262890683122, 1.000000000000000000, 0.9659258262890683122, 1.000000000000000000, 0.9659258262890683122, 1.000000000000000000, 0.9659258262890683122, 1.000000000000000000, 0.9659258262890683122, 1.000000000000000000, 0.9659258262890683122, 1.000000000000000000, 0.9659258262890683122, 1.000000000000000000, 0.9659258262890683122, 1.000000000000000000, 0.9659258262890683122, 1.000000000000000000, 0.9659258262890683122, 1.000000000000000000, 0.9659258262890683122, 1.000000000000000000, 0.9659258262890683122, 1.000000000000000000, 0.9659258262890683122, 1.000000000000000000, 0.9659258262890683122, 1.000000000000000000, 0.9659258262890683122, 1.000000000000000000, 0.9659258262890683122, 1.000000000000000000, 0.9659258262890683122, 1.000000000000000000, 0.9659258262890683122, 1.000000000000000000, 0.9659258262890683122, 1.000000000000000000, 0.9659258262890683122, 1.000000000000000000, 0.9659258262890683122, 1.000000000000000000, 0.9659258262890683122, 1.000000000000000000, 0.9659258262890683122, 1.000000000000000000, 0.9659258262890683122, 1.000000000000000000, 0.9659258262890683122, 1.000000000000000000, 0.9659258262890683122, 1.000000000000000000, 0.9659258262890683122, 1.000000000000000000, 0.9659258262890683122, 1.000000000000000000, 0.9659258262890683122, 1.000000000000000000, 0.9659258262890683122, 1.000000000000000000, 0.9659258262890683122, 1.000000000000000000, 0.9659258262890683122, 1.000000000000000000, 0.9659258262890683122, 1.000000000000000000, 0.9659258262890683122, 1.000000000000000000, 0.9659258262890683122, 1.000000000000000000, 0.9659258262890683122, 1.000000000000000000, 0.9659258262890683122, 1.000000000000000000, 0.9659258262890683122, 1.000000000000000000, 0.9659258262890683122, 1.000000000000000000, 0.9659258262890683122, 1.000000000000000000, 0.9659258262890683122, 1.000000000000000000, 0.9659258262890683122, 1.000000000000000000, 0.9659258262890683122, 1.000000000000000000, 0.9659258262890683122, 1.000000000000000000, 0.9659258262890683122, 1.000000000000000000, 0.9659258262890683122, 1.000000000000000000, 0.9659258262890683122, 1.000000000000000000, 0.9659258262890683122, 1.000000000000000000, 0.9659258262890683122, 1.000000000000000000, 0.9659258262890683122, 1.000000000000000000, 0.9659258262890683122, 1.000000000000000000, 0.9659258262890683122, 1.000000000000000000, 0.9659258262890683122, 1.000000000000000000, 0.9659258262890683122, 1.000000000000000000, 0.9659258262890683122, 1.000000000000000000, 0.9659258262890683122, 1.000000000000000000, 0.9659258262890683122, 1.000000000000000000, 0.9659258262890683122, 1.000000000000000000, 0.9659258262890683122, 1.000000000000000000, 0.9659258262890683122, 1.000000000000000000, 0.9659258262890683122, 1.000000000000000000, 0.9659258262890683122, 1.000000000000000000, 0.9659258262890683122, 1.000000000000000000, 0.9659258262890683122, 1.000000000000000000, 0.9659258262890683122, 1.000000000000000000, 0.9659258262890683122, 1.000000000000000000, 0.9659258262890683122, 1.000000000000000000, 0.9659258262890683122, 1.000000000000000000, 0.9659258262890683122, 1.000000000000000000, 0.9659258262890683122, 1.000000000000000000, 0.9659258262890683122, 1.000000000000000000, 0.9659258262890683122, 1.000000000000000000, 0.9659258262890683122, 1.000000000000000000, 0.9659258262890683122, 1.000000000000000000, 0.9659258262890683122, 1.000000000000000000, 0.9659258262890683122, 1.000000000000000000, 0.9659258262890683122, 1.000000000000000000, 0.9659258262890683122, 1.000000000000000000, 0.9659258262890683122, 1.000000000000000000) ) ) 
 REPRESENTATION_ITEM ( '' )  SURFACE ( )  );
#17017 = ADVANCED_FACE ( 'NONE', ( #16006, #2659, #8270, #15722, #13040, #3851, #8640, #14429, #10098, #9814, #11570, #6883, #8454 ), #3943, .F. ) ;
#17018 = CARTESIAN_POINT ( 'NONE',  ( -24.00000000000000711, 53.00000000000000711, -19.00000000000000000 ) ) ;
#17019 = EDGE_CURVE ( 'NONE', #11126, #4048, #9909, .T. ) ;
#17020 = CARTESIAN_POINT ( 'NONE',  ( -10.58745947852649927, -21.64274437364853654, 20.88867750791695954 ) ) ;
#17021 = PLANE ( 'NONE',  #7346 ) ;
#17022 = CARTESIAN_POINT ( 'NONE',  ( -9.999999999999994671, -24.16482700510257686, 26.57617750791695954 ) ) ;
#17023 = PLANE ( 'NONE',  #12176 ) ;
#17024 = CARTESIAN_POINT ( 'NONE',  ( -19.41254052147350961, -21.64274437364857562, 26.36132249208304401 ) ) ;
#17025 = CARTESIAN_POINT ( 'NONE',  ( -0.8561741729129461742, 66.06698729999999387, 48.80000000109247082 ) ) ;
#17026 = CARTESIAN_POINT ( 'NONE',  ( -41.00000000000000711, 110.0000000000000000, -44.00000000000000000 ) ) ;
#17027 = PLANE ( 'NONE',  #10690 ) ;
#17028 = CARTESIAN_POINT ( 'NONE',  ( -41.00000000000000711, 53.00000000000000711, 6.999999999999999112 ) ) ;
#17029 = CARTESIAN_POINT ( 'NONE',  ( 2.066987300000001415, 64.00000000000000000, 46.95000000109246940 ) ) ;
#17030 = DIRECTION ( 'NONE',  ( -0.000000000000000000, 0.7071067811865456854, 0.7071067811865493491 ) ) ;
#17031 = VERTEX_POINT ( 'NONE', #6797 ) ;
#17032 = VERTEX_POINT ( 'NONE', #17285 ) ;
#17033 = CARTESIAN_POINT ( 'NONE',  ( -21.95583473709189803, -26.04047135212049469, 36.20507249208304046 ) ) ;
#17034 = FILL_AREA_STYLE_COLOUR ( '', #5163 ) ;
#17035 = CARTESIAN_POINT ( 'NONE',  ( -14.83517299489735741, -28.99999999999998224, 8.861322492083040459 ) ) ;
#17036 = CARTESIAN_POINT ( 'NONE',  ( -17.95583473709191580, -23.03132541760400898, 29.41992750791696665 ) ) ;
#17037 = CARTESIAN_POINT ( 'NONE',  ( 1.300000000000000044, 1.690103923579304181E-15, 1.280000000000000249 ) ) ;
#17038 = CARTESIAN_POINT ( 'NONE',  ( -8.044165262908093084, -21.95952864787946979, 17.83007249208304046 ) ) ;
#17039 = CARTESIAN_POINT ( 'NONE',  ( -2.066987300000001859, 64.85617417291294373, 47.10000000109246798 ) ) ;
#17040 = LINE ( 'NONE', #9570, #4716 ) ;
#17041 = ORIENTED_EDGE ( 'NONE', *, *, #13416, .T. ) ;
#17042 = ORIENTED_EDGE ( 'NONE', *, *, #18009, .T. ) ;
#17043 = DIRECTION ( 'NONE',  ( -0.000000000000000000, 1.000000000000000000, -0.000000000000000000 ) ) ;
#17044 = DIRECTION ( 'NONE',  ( 1.000000000000000000, 0.000000000000000000, 2.081668171172167774E-16 ) ) ;
#17045 = DIRECTION ( 'NONE',  ( -1.000000000000000000, -0.000000000000000000, -0.000000000000000000 ) ) ;
#17046 = ADVANCED_FACE ( 'NONE', ( #15901 ), #6701, .T. ) ;
#17047 = DIRECTION ( 'NONE',  ( -0.000000000000000000, -0.000000000000000000, -1.000000000000000000 ) ) ;
#17048 = CARTESIAN_POINT ( 'NONE',  ( 32.49999999999998579, -6.000000000000000000, 42.49999999999997868 ) ) ;
#17049 = DIRECTION ( 'NONE',  ( -0.000000000000000000, 0.000000000000000000, -1.000000000000000000 ) ) ;
#17050 = VERTEX_POINT ( 'NONE', #4147 ) ;
#17051 = VERTEX_POINT ( 'NONE', #2376 ) ;
#17052 = CARTESIAN_POINT ( 'NONE',  ( -21.14459132904236327, -27.35725562635143149, 34.01367750791695244 ) ) ;
#17053 = VERTEX_POINT ( 'NONE', #14240 ) ;
#17055 = ORIENTED_EDGE ( 'NONE', *, *, #14501, .T. ) ;
#17054 = ORIENTED_EDGE ( 'NONE', *, *, #12620, .T. ) ;
#17056 = CARTESIAN_POINT ( 'NONE',  ( -14.83517299489736985, -26.99999999999998579, 35.11132249208304756 ) ) ;
#17057 = CARTESIAN_POINT ( 'NONE',  ( -9.996306089212364299, -29.24501739517662813, 11.48242750791695777 ) ) ;
#17058 = STYLED_ITEM ( 'NONE', ( #11403 ), #14596 ) ;
#17059 = EDGE_CURVE ( 'NONE', #4614, #13503, #11289, .T. ) ;
#17060 = VECTOR ( 'NONE', #9829, 1000.000000000000000 ) ;
#17061 = CARTESIAN_POINT ( 'NONE',  ( -4.999999999999996447, -32.00000000000000000, 9.500000000000001776 ) ) ;
#17062 = CARTESIAN_POINT ( 'NONE',  ( 2.500000000000002220, 62.96446609406726935, 46.45000000218495018 ) ) ;
#17063 = CARTESIAN_POINT ( 'NONE',  ( 8.000000000000014211, 60.00000000000000711, 45.00000000000000000 ) ) ;
#17064 = VERTEX_POINT ( 'NONE', #721 ) ;
#17065 = EDGE_CURVE ( 'NONE', #9098, #15107, #18857, .T. ) ;
#17066 = CARTESIAN_POINT ( 'NONE',  ( -13.64274437364856141, -26.68048971390460622, 27.45117750791696309 ) ) ;
#17067 =( NAMED_UNIT ( * ) PLANE_ANGLE_UNIT ( ) SI_UNIT ( $, .RADIAN. ) );
#17068 = ORIENTED_EDGE ( 'NONE', *, *, #8741, .F. ) ;
#17069 = CARTESIAN_POINT ( 'NONE',  ( -37.50000000000002132, -6.000000000000000000, 44.99999999999997868 ) ) ;
#17070 = ORIENTED_EDGE ( 'NONE', *, *, #2528, .T. ) ;
#17071 = LINE ( 'NONE', #3633, #8193 ) ;
#17072 = CARTESIAN_POINT ( 'NONE',  ( 0.000000000000000000, 64.00000000000000000, 49.99999999999999289 ) ) ;
#17073 = CARTESIAN_POINT ( 'NONE',  ( -24.00000000000000000, 53.00000000000000711, 30.00000000000000000 ) ) ;
#17074 = DIRECTION ( 'NONE',  ( 0.000000000000000000, 0.000000000000000000, -1.000000000000000000 ) ) ;
#17075 = CARTESIAN_POINT ( 'NONE',  ( 2.066987300000001859, 64.85617417291294373, 47.60000000109246798 ) ) ;
#17076 = CARTESIAN_POINT ( 'NONE',  ( 1.461580736456473684, 65.46158073645646880, 48.65000000109247225 ) ) ;
#17077 = CARTESIAN_POINT ( 'NONE',  ( 1.000000000000000222, -28.00000000000000000, 4.500000000000000888 ) ) ;
#17078 = CARTESIAN_POINT ( 'NONE',  ( 1.767766952966369987, 65.76776695296638309, 49.69999999999999574 ) ) ;
#17079 = AXIS2_PLACEMENT_3D ( 'NONE', #14919, #5897, #3050 ) ;
#17080 = PLANE ( 'NONE',  #13307 ) ;
#17081 = ORIENTED_EDGE ( 'NONE', *, *, #14772, .T. ) ;
#17082 = CARTESIAN_POINT ( 'NONE',  ( -17.35725562635144215, -19.58745947852648683, 24.82617750791695954 ) ) ;
#17083 = CARTESIAN_POINT ( 'NONE',  ( -3.155775640247338920, -41.39960408384398249, 1.500000000000000000 ) ) ;
#17084 = ORIENTED_EDGE ( 'NONE', *, *, #5201, .F. ) ;
#17085 = CARTESIAN_POINT ( 'NONE',  ( -18.78091578003892081, -20.46040770435013556, 26.58007249208304401 ) ) ;
#17086 = EDGE_CURVE ( 'NONE', #12041, #184, #19038, .T. ) ;
#17087 = CARTESIAN_POINT ( 'NONE',  ( -18.04416526290808775, -23.36097942780924441, 31.39257249208304401 ) ) ;
#17088 =( NAMED_UNIT ( * ) SI_UNIT ( $, .STERADIAN. ) SOLID_ANGLE_UNIT ( ) );
#17089 = VERTEX_POINT ( 'NONE', #12760 ) ;
#17090 = VECTOR ( 'NONE', #1269, 1000.000000000000000 ) ;
#17091 = CARTESIAN_POINT ( 'NONE',  ( -40.00000000000000711, 113.0000000000000000, -50.00000000000000000 ) ) ;
#17092 = EDGE_LOOP ( 'NONE', ( #7442, #17757, #4975, #16266, #18348 ) ) ;
#17093 = DIRECTION ( 'NONE',  ( -0.000000000000000000, -0.000000000000000000, -1.000000000000000000 ) ) ;
#17094 = ADVANCED_FACE ( 'NONE', ( #18755 ), #8361, .T. ) ;
#17095 = LINE ( 'NONE', #17186, #16752 ) ;
#17096 = CYLINDRICAL_SURFACE ( 'NONE', #14749, 2.500000000000001776 ) ;
#17097 = MANIFOLD_SOLID_BREP ( 'M5 Clearance Hole1', #19180 ) ;
#17098 = CARTESIAN_POINT ( 'NONE',  ( -1.530808498934192803E-16, 66.50000000000000000, 46.59999999999999432 ) ) ;
#17099 = DIRECTION ( 'NONE',  ( 1.000000000000000000, 0.000000000000000000, 9.251858538542970348E-17 ) ) ;
#17100 = AXIS2_PLACEMENT_3D ( 'NONE', #18332, #3419, #7941 ) ;
#17101 = CARTESIAN_POINT ( 'NONE',  ( -10.00000000000000000, -35.50000000000000711, 7.999999999999996447 ) ) ;
#17102 = VECTOR ( 'NONE', #742, 1000.000000000000000 ) ;
#17103 = EDGE_CURVE ( 'NONE', #5273, #15869, #12011, .T. ) ;
#17104 = ORIENTED_EDGE ( 'NONE', *, *, #303, .F. ) ;
#17105 = CARTESIAN_POINT ( 'NONE',  ( -13.82508104294698192, -29.04416526290806644, 32.91992750791695954 ) ) ;
#17106 = CARTESIAN_POINT ( 'NONE',  ( -2.500000000000001776, 65.03553390593273775, 45.25000000218494733 ) ) ;
#17107 = CARTESIAN_POINT ( 'NONE',  ( -12.64274437364858628, -19.58745947852646552, 32.92382249208304046 ) ) ;
#17108 = DIRECTION ( 'NONE',  ( 1.000000000000000000, -0.000000000000000000, -0.000000000000000000 ) ) ;
#17109 = CARTESIAN_POINT ( 'NONE',  ( -16.50457296725820555, -28.95583473709189448, 17.60742750791695599 ) ) ;
#17110 = DIRECTION ( 'NONE',  ( 0.000000000000000000, 1.000000000000000000, 0.000000000000000000 ) ) ;
#17111 = AXIS2_PLACEMENT_3D ( 'NONE', #2661, #1008, #14432 ) ;
#17112 = CARTESIAN_POINT ( 'NONE',  ( -19.95583473709191225, -22.49542703274176603, 29.41992750791695599 ) ) ;
#17113 = CARTESIAN_POINT ( 'NONE',  ( -2.500000000000001776, 64.00000000000000000, 46.79999999999999716 ) ) ;
#17114 = CARTESIAN_POINT ( 'NONE',  ( -16.50457296725825174, -19.04416526290807354, 27.01757249208304046 ) ) ;
#17115 = AXIS2_PLACEMENT_3D ( 'NONE', #15502, #1686, #7768 ) ;
#17116 = CARTESIAN_POINT ( 'NONE',  ( 0.8561741729129472844, 61.93301270000000613, 46.00000000109245946 ) ) ;
#17117 = DIRECTION ( 'NONE',  ( 0.000000000000000000, -1.000000000000000000, 0.000000000000000000 ) ) ;
#17118 = CARTESIAN_POINT ( 'NONE',  ( 46.99999999999997868, 30.00000000000000355, 59.99999999999999289 ) ) ;
#17119 = LINE ( 'NONE', #2120, #15237 ) ;
#17120 = CARTESIAN_POINT ( 'NONE',  ( -2.066987300000001415, 64.00000000000000000, 48.15000000109247225 ) ) ;
#17121 = CARTESIAN_POINT ( 'NONE',  ( 5.799999999999985612, 29.47747564417429444, 56.65425233947099315 ) ) ;
#17122 = EDGE_LOOP ( 'NONE', ( #4189, #969, #1080, #19114, #10720, #13121, #9949, #5859 ) ) ;
#17123 = CARTESIAN_POINT ( 'NONE',  ( -17.04047135212050890, -17.04416526290807710, 37.51757249208304046 ) ) ;
#17124 = AXIS2_PLACEMENT_3D ( 'NONE', #1475, #1276, #7344 ) ;
#17125 = AXIS2_PLACEMENT_3D ( 'NONE', #11594, #14453, #1027 ) ;
#17126 = CARTESIAN_POINT ( 'NONE',  ( 3.399999999999996803, 29.65425233947093631, 56.83102903476762435 ) ) ;
#17127 = CARTESIAN_POINT ( 'NONE',  ( -16.35725562635142794, -21.31951028609535470, 35.32617750791695244 ) ) ;
#17128 = CARTESIAN_POINT ( 'NONE',  ( -25.00000000000001421, -6.000000000000000000, 42.49999999999997868 ) ) ;
#17129 = CARTESIAN_POINT ( 'NONE',  ( -15.16482700510264436, -16.99999999999997868, 21.98632249208304046 ) ) ;
#17130 = CARTESIAN_POINT ( 'NONE',  ( -1.461580736456473462, 62.53841926354353120, 45.65000000109247225 ) ) ;
#17131 = ORIENTED_EDGE ( 'NONE', *, *, #8254, .T. ) ;
#17132 = EDGE_LOOP ( 'NONE', ( #15701, #3116, #2748, #15439 ) ) ;
#17133 = CARTESIAN_POINT ( 'NONE',  ( -1.485306817036799787, -16.78846153846157918, -16.05769230769231015 ) ) ;
#17134 = CYLINDRICAL_SURFACE ( 'NONE', #4113, 2.500000000000002220 ) ;
#17135 = CARTESIAN_POINT ( 'NONE',  ( 3.796994071234847710E-16, 61.93301269999999903, 47.35000000109246798 ) ) ;
#17136 = CARTESIAN_POINT ( 'NONE',  ( 49.99999999999998579, 3.000000000000000000, 59.99999999999997868 ) ) ;
#17137 = PRESENTATION_LAYER_ASSIGNMENT (  '', '', ( #5247 ) ) ;
#17138 = CARTESIAN_POINT ( 'NONE',  ( -1.461580736456473462, 62.53841926354353120, 45.05000000109246372 ) ) ;
#17139 = CARTESIAN_POINT ( 'NONE',  ( -41.00000000000000711, 53.00000000000000711, 21.00000000000000000 ) ) ;
#17140 = LINE ( 'NONE', #3703, #9567 ) ;
#17141 = ORIENTED_EDGE ( 'NONE', *, *, #15327, .T. ) ;
#17142 = ORIENTED_EDGE ( 'NONE', *, *, #11190, .T. ) ;
#17143 = CARTESIAN_POINT ( 'NONE',  ( -20.97976432393977575, -20.35725562635143504, 24.38867750791695954 ) ) ;
#17144 =( NAMED_UNIT ( * ) PLANE_ANGLE_UNIT ( ) SI_UNIT ( $, .RADIAN. ) );
#17145 = VERTEX_POINT ( 'NONE', #10293 ) ;
#17147 = EDGE_LOOP ( 'NONE', ( #7429, #12718, #10081, #1749 ) ) ;
#17146 = ORIENTED_EDGE ( 'NONE', *, *, #4129, .F. ) ;
#17148 = CARTESIAN_POINT ( 'NONE',  ( -17.51566270880199738, -25.64274437364856496, 25.48632249208304401 ) ) ;
#17149 = ADVANCED_FACE ( 'NONE', ( #16191 ), #18065, .T. ) ;
#17150 = EDGE_CURVE ( 'NONE', #2227, #869, #3156, .T. ) ;
#17151 = CARTESIAN_POINT ( 'NONE',  ( -14.83517299489740715, -16.99999999999997868, 14.76367750791695777 ) ) ;
#17152 = DIRECTION ( 'NONE',  ( 0.000000000000000000, -1.000000000000000000, 0.000000000000000000 ) ) ;
#17153 = CARTESIAN_POINT ( 'NONE',  ( -2.500000000000001776, 65.03553390593273775, 46.85000000218494165 ) ) ;
#17154 = DIRECTION ( 'NONE',  ( 0.000000000000000000, -1.000000000000000000, -0.000000000000000000 ) ) ;
#17155 = ORIENTED_EDGE ( 'NONE', *, *, #9935, .T. ) ;
#17156 = CARTESIAN_POINT ( 'NONE',  ( -11.99999999999999289, -24.16482700510258752, 31.82617750791696309 ) ) ;
#17157 = ADVANCED_FACE ( 'NONE', ( #1188 ), #1300, .F. ) ;
#17158 = DIRECTION ( 'NONE',  ( 0.000000000000000000, 0.000000000000000000, -1.000000000000000000 ) ) ;
#17159 = ORIENTED_EDGE ( 'NONE', *, *, #12935, .T. ) ;
#17160 = DIRECTION ( 'NONE',  ( -0.5773502691896311712, -0.8164965809277222597, 0.000000000000000000 ) ) ;
#17161 = ORIENTED_EDGE ( 'NONE', *, *, #16077, .T. ) ;
#17162 = CYLINDRICAL_SURFACE ( 'NONE', #50, 2.500000000000001776 ) ;
#17163 = CARTESIAN_POINT ( 'NONE',  ( 1.000000000000001998, -32.00000000000000000, 9.500000000000001776 ) ) ;
#17164 = DIRECTION ( 'NONE',  ( 0.000000000000000000, 0.000000000000000000, -1.000000000000000000 ) ) ;
#17165 = EDGE_CURVE ( 'NONE', #18948, #15097, #19140, .T. ) ;
#17166 = CARTESIAN_POINT ( 'NONE',  ( -0.8561741729129465073, 61.93301270000000613, 47.30000000109247082 ) ) ;
#17167 = CARTESIAN_POINT ( 'NONE',  ( 0.8561741729129460632, 66.06698730000000808, 49.50000000109246656 ) ) ;
#17168 = LINE ( 'NONE', #9703, #5342 ) ;
#17169 = DIRECTION ( 'NONE',  ( 0.000000000000000000, 0.000000000000000000, 1.000000000000000000 ) ) ;
#17170 = CARTESIAN_POINT ( 'NONE',  ( -50.00000000000002132, 118.0000000000000142, 40.49999999999997868 ) ) ;
#17171 = ORIENTED_EDGE ( 'NONE', *, *, #16409, .F. ) ;
#17172 = ORIENTED_EDGE ( 'NONE', *, *, #13342, .T. ) ;
#17173 = ADVANCED_FACE ( 'NONE', ( #7570 ), #7368, .F. ) ;
#17174 = CARTESIAN_POINT ( 'NONE',  ( -20.04416526290808065, -25.17491895705300209, 23.73242750791694888 ) ) ;
#17175 = CARTESIAN_POINT ( 'NONE',  ( 50.00000000000000000, 33.00000000000000000, 44.99999999999999289 ) ) ;
#17176 = ORIENTED_EDGE ( 'NONE', *, *, #12727, .F. ) ;
#17177 = CARTESIAN_POINT ( 'NONE',  ( -19.95583473709190514, -25.50457296725822687, 25.70507249208304756 ) ) ;
#17178 = CARTESIAN_POINT ( 'NONE',  ( 2.492551403682577771, 31.20336399182262710, 54.92836399182266405 ) ) ;
#17179 = ADVANCED_FACE ( 'NONE', ( #10593 ), #8730, .T. ) ;
#17180 = CARTESIAN_POINT ( 'NONE',  ( -12.68318583509882380, -26.07549068051207541, 34.45507249208304046 ) ) ;
#17181 = DIRECTION ( 'NONE',  ( 0.000000000000000000, 0.5000000000000011102, 0.8660254037844379305 ) ) ;
#17182 = ORIENTED_EDGE ( 'NONE', *, *, #10181, .T. ) ;
#17183 = LINE ( 'NONE', #14420, #5940 ) ;
#17184 = EDGE_LOOP ( 'NONE', ( #9840, #2145, #8439, #1085 ) ) ;
#17185 = CARTESIAN_POINT ( 'NONE',  ( -41.00000000000000711, 53.00000000000000711, -44.00000000000000000 ) ) ;
#17186 = CARTESIAN_POINT ( 'NONE',  ( 2.500000000000001776, 64.00000000000000000, 49.99999999999999289 ) ) ;
#17187 = VECTOR ( 'NONE', #14642, 1000.000000000000000 ) ;
#17188 = DIRECTION ( 'NONE',  ( -0.000000000000000000, -0.000000000000000000, -1.000000000000000000 ) ) ;
#17189 = EDGE_CURVE ( 'NONE', #13388, #2239, #13541, .T. ) ;
#17190 = EDGE_CURVE ( 'NONE', #15646, #1350, #17964, .T. ) ;
#17191 = CARTESIAN_POINT ( 'NONE',  ( -41.00000000000000711, 113.0000000000000000, 30.00000000000000000 ) ) ;
#17192 =( LENGTH_UNIT ( ) NAMED_UNIT ( * ) SI_UNIT ( .MILLI., .METRE. ) );
#17193 = EDGE_CURVE ( 'NONE', #5763, #5764, #13142, .T. ) ;
#17194 = LINE ( 'NONE', #3946, #12403 ) ;
#17195 = VECTOR ( 'NONE', #14306, 1000.000000000000000 ) ;
#17196 = CARTESIAN_POINT ( 'NONE',  ( 37.49999999999999289, -6.000000000000000000, 47.49999999999997868 ) ) ;
#17197 = ORIENTED_EDGE ( 'NONE', *, *, #5966, .T. ) ;
#17198 = ADVANCED_FACE ( 'NONE', ( #10196 ), #11866, .T. ) ;
#17199 = VECTOR ( 'NONE', #4575, 1000.000000000000114 ) ;
#17200 = CARTESIAN_POINT ( 'NONE',  ( -11.46040770435012668, -27.78091578003887463, 32.48242750791695954 ) ) ;
#17201 = CARTESIAN_POINT ( 'NONE',  ( -2.066987300000001859, 64.85617417291294373, 47.90000000109247225 ) ) ;
#17202 = CARTESIAN_POINT ( 'NONE',  ( -13.49542703274174116, -28.95583473709188738, 34.89257249208304046 ) ) ;
#17203 = LINE ( 'NONE', #4864, #7913 ) ;
#17204 = CARTESIAN_POINT ( 'NONE',  ( -19.99999999999999645, -23.83517299489738051, 23.95117750791695954 ) ) ;
#17205 = DIRECTION ( 'NONE',  ( 0.000000000000000000, 1.000000000000000000, -0.000000000000000000 ) ) ;
#17207 = CARTESIAN_POINT ( 'NONE',  ( -19.95583473709191225, -22.49542703274176603, 34.66992750791695244 ) ) ;
#17206 = VECTOR ( 'NONE', #6785, 1000.000000000000000 ) ;
#17208 = CARTESIAN_POINT ( 'NONE',  ( -1.035533905932738641, 66.50000000000000000, 46.75000000218494733 ) ) ;
#17209 = CARTESIAN_POINT ( 'NONE',  ( -10.04416526290808598, -22.49542703274172695, 28.33007249208304401 ) ) ;
#17210 = ADVANCED_FACE ( 'NONE', ( #9031 ), #119, .F. ) ;
#17211 = CARTESIAN_POINT ( 'NONE',  ( -2.500000000000001776, 64.00000000000000000, 49.99999999999999289 ) ) ;
#17212 = CARTESIAN_POINT ( 'NONE',  ( -41.00000000000000711, 53.00000000000000711, -24.49999999999999645 ) ) ;
#17213 = VECTOR ( 'NONE', #1017, 1000.000000000000000 ) ;
#17214 = VECTOR ( 'NONE', #15279, 1000.000000000000000 ) ;
#17215 = LINE ( 'NONE', #5350, #7332 ) ;
#17216 = CARTESIAN_POINT ( 'NONE',  ( -2.066987300000001415, 64.00000000000000000, 44.95000000109246940 ) ) ;
#17217 = CARTESIAN_POINT ( 'NONE',  ( 37.49999999999999289, 0.000000000000000000, 24.99999999999998579 ) ) ;
#17218 = EDGE_LOOP ( 'NONE', ( #6970, #6509, #13694, #7446 ) ) ;
#17219 = AXIS2_PLACEMENT_3D ( 'NONE', #18668, #17093, #3845 ) ;
#17220 = CARTESIAN_POINT ( 'NONE',  ( -1.461580736456473906, 65.46158073645646880, 46.25000000109247367 ) ) ;
#17221 = CARTESIAN_POINT ( 'NONE',  ( -15.16482700510260706, -26.99999999999998579, 27.88867750791696309 ) ) ;
#17222 = CARTESIAN_POINT ( 'NONE',  ( -1.035533905932738641, 66.50000000000000000, 49.04999999999999716 ) ) ;
#17223 = CARTESIAN_POINT ( 'NONE',  ( -7.955834737091903364, -25.71081734191518464, 28.76757249208303691 ) ) ;
#17224 = AXIS2_PLACEMENT_3D ( 'NONE', #12057, #10389, #2749 ) ;
#17225 = CARTESIAN_POINT ( 'NONE',  ( -0.8561741729129461742, 66.06698729999999387, 45.40000000109246514 ) ) ;
#17226 = ORIENTED_EDGE ( 'NONE', *, *, #14218, .T. ) ;
#17227 = LINE ( 'NONE', #11326, #2200 ) ;
#17228 = DIRECTION ( 'NONE',  ( -1.000000000000000000, -0.000000000000000000, -0.000000000000000000 ) ) ;
#17229 = CIRCLE ( 'NONE', #14093, 10.00000000000000178 ) ;
#17230 = EDGE_CURVE ( 'NONE', #8073, #18948, #17662, .T. ) ;
#17231 = CARTESIAN_POINT ( 'NONE',  ( 2.066987300000001415, 64.85617417291294373, 46.80000000109247082 ) ) ;
#17232 = DIRECTION ( 'NONE',  ( -1.000000000000000000, 0.000000000000000000, 0.000000000000000000 ) ) ;
#17233 = DIRECTION ( 'NONE',  ( -1.000000000000000000, 0.000000000000000000, -0.000000000000000000 ) ) ;
#17234 = DIRECTION ( 'NONE',  ( 2.220446049250313081E-16, 0.7071067811865452413, 0.7071067811865497932 ) ) ;
#17235 = VECTOR ( 'NONE', #13016, 1000.000000000000000 ) ;
#17236 = FACE_OUTER_BOUND ( 'NONE', #15297, .T. ) ;
#17237 = ORIENTED_EDGE ( 'NONE', *, *, #12367, .F. ) ;
#17238 = VERTEX_POINT ( 'NONE', #13240 ) ;
#17239 = CARTESIAN_POINT ( 'NONE',  ( -18.35725562635144925, -17.85540867095761186, 35.32617750791695244 ) ) ;
#17240 = VERTEX_POINT ( 'NONE', #19236 ) ;
#17242 = ORIENTED_EDGE ( 'NONE', *, *, #4130, .F. ) ;
#17241 = ORIENTED_EDGE ( 'NONE', *, *, #4140, .T. ) ;
#17243 = CARTESIAN_POINT ( 'NONE',  ( -12.68318583509882380, -26.07549068051207541, 34.45507249208304046 ) ) ;
#17244 = CARTESIAN_POINT ( 'NONE',  ( -18.35725562635144925, -17.85540867095761186, 30.07617750791695599 ) ) ;
#17245 = VECTOR ( 'NONE', #13427, 1000.000000000000000 ) ;
#17246 = CARTESIAN_POINT ( 'NONE',  ( 1.767766952966370653, 62.23223304703363112, 46.40000000218494591 ) ) ;
#17247 = LINE ( 'NONE', #9960, #18486 ) ;
#17248 = ORIENTED_EDGE ( 'NONE', *, *, #500, .T. ) ;
#17249 = CARTESIAN_POINT ( 'NONE',  ( -17.31681416490115311, -26.07549068051209318, 33.79492750791695954 ) ) ;
#17250 = AXIS2_PLACEMENT_3D ( 'NONE', #15853, #11332, #17324 ) ;
#17251 = CARTESIAN_POINT ( 'NONE',  ( -24.00000000000000000, 113.0000000000000000, 30.00000000000000000 ) ) ;
#17252 = VERTEX_POINT ( 'NONE', #11768 ) ;
#17253 = DIRECTION ( 'NONE',  ( 6.216479319370943891E-15, -1.000000000000000000, 0.000000000000000000 ) ) ;
#17254 = VERTEX_POINT ( 'NONE', #17764 ) ;
#17255 = DIRECTION ( 'NONE',  ( 0.000000000000000000, 0.000000000000000000, 1.000000000000000000 ) ) ;
#17256 = DIRECTION ( 'NONE',  ( -0.000000000000000000, 0.000000000000000000, 1.000000000000000000 ) ) ;
#17257 = LINE ( 'NONE', #3635, #14692 ) ;
#17258 = CARTESIAN_POINT ( 'NONE',  ( -2.066987300000001415, 64.00000000000000000, 45.55000000109246372 ) ) ;
#17259 = VECTOR ( 'NONE', #4025, 1000.000000000000000 ) ;
#17260 = CARTESIAN_POINT ( 'NONE',  ( -2.066987300000001415, 64.00000000000000000, 48.15000000109247225 ) ) ;
#17261 = CARTESIAN_POINT ( 'NONE',  ( 14.99999999999998579, 73.00000000000001421, 26.99999999999997158 ) ) ;
#17262 = AXIS2_PLACEMENT_3D ( 'NONE', #16185, #14715, #7271 ) ;
#17263 = DIRECTION ( 'NONE',  ( 0.1648270051026194671, 0.000000000000000000, -0.9863224920830413467 ) ) ;
#17264 = PLANE ( 'NONE',  #10490 ) ;
#17265 = VERTEX_POINT ( 'NONE', #7669 ) ;
#17266 = VERTEX_POINT ( 'NONE', #1889 ) ;
#17267 = CARTESIAN_POINT ( 'NONE',  ( -10.75228648362910100, -26.64274437364854009, 37.51367750791695954 ) ) ;
#17268 = CIRCLE ( 'NONE', #12580, 2.500000000000002220 ) ;
#17269 = CARTESIAN_POINT ( 'NONE',  ( -2.500000000000001776, 64.00000000000000000, 49.99999999999999289 ) ) ;
#17270 = VERTEX_POINT ( 'NONE', #18164 ) ;
#17271 = CARTESIAN_POINT ( 'NONE',  ( -18.53959229564982536, -27.78091578003890660, 35.76757249208302625 ) ) ;
#17272 = AXIS2_PLACEMENT_3D ( 'NONE', #12427, #3516, #9483 ) ;
#17273 = DIRECTION ( 'NONE',  ( 0.000000000000000000, 0.7071067811865456854, 0.7071067811865494601 ) ) ;
#17274 = CARTESIAN_POINT ( 'NONE',  ( -16.35725562635141372, -26.68048971390461332, 30.29882249208304401 ) ) ;
#17275 = PLANE ( 'NONE',  #3793 ) ;
#17276 = VERTEX_POINT ( 'NONE', #4933 ) ;
#17277 = VECTOR ( 'NONE', #739, 1000.000000000000000 ) ;
#17278 = LINE ( 'NONE', #9720, #4376 ) ;
#17279 = ORIENTED_EDGE ( 'NONE', *, *, #14860, .T. ) ;
#17280 = DIRECTION ( 'NONE',  ( -5.782411586589357392E-17, 0.000000000000000000, -1.000000000000000000 ) ) ;
#17281 = DIRECTION ( 'NONE',  ( -1.156482317317871478E-16, 1.000000000000000000, 0.000000000000000000 ) ) ;
#17282 = AXIS2_PLACEMENT_3D ( 'NONE', #6941, #4297, #14786 ) ;
#17283 = CARTESIAN_POINT ( 'NONE',  ( 2.500000000000001776, 64.00000000000000000, 49.99999999999999289 ) ) ;
#17284 = ADVANCED_FACE ( 'NONE', ( #9518 ), #17080, .T. ) ;
#17285 = CARTESIAN_POINT ( 'NONE',  ( 20.00000000000000355, -32.00000000000000711, 0.000000000000000000 ) ) ;
#17286 = CARTESIAN_POINT ( 'NONE',  ( -41.99999999999997868, 139.6861997365471950, 51.99999999999997868 ) ) ;
#17287 = CARTESIAN_POINT ( 'NONE',  ( -15.00000000000000000, 35.00000000000000000, 37.00000000000000000 ) ) ;
#17288 = CARTESIAN_POINT ( 'NONE',  ( 46.99999999999998579, 115.0000000000000000, 37.49999999999997868 ) ) ;
#17289 = ORIENTED_EDGE ( 'NONE', *, *, #8395, .F. ) ;
#17290 =( BOUNDED_CURVE ( )  B_SPLINE_CURVE ( 2, ( #11953, #10273, #8712, #9110, #5882 ),
 .UNSPECIFIED., .F., .F. ) 
 B_SPLINE_CURVE_WITH_KNOTS ( ( 3, 2, 3 ),
 ( 0.8571428571428569843, 0.8750000000000000000, 0.8928571428571429047 ),
 .UNSPECIFIED. ) 
 CURVE ( )  GEOMETRIC_REPRESENTATION_ITEM ( )  RATIONAL_B_SPLINE_CURVE ( ( 1.000000000000000444, 0.9238795325112862944, 1.000000000000000000, 0.9238795325112867385, 1.000000000000000000 ) ) 
 REPRESENTATION_ITEM ( '' )  );
#17291 = VECTOR ( 'NONE', #247, 1000.000000000000000 ) ;
#17292 = CARTESIAN_POINT ( 'NONE',  ( -15.16482700510259640, -28.99999999999998224, 27.88867750791695954 ) ) ;
#17293 = CARTESIAN_POINT ( 'NONE',  ( -1.461580736456473462, 62.53841926354353120, 47.25000000109247367 ) ) ;
#17294 = CARTESIAN_POINT ( 'NONE',  ( -11.21908421996106320, -27.53959229564982181, 39.70507249208304046 ) ) ;
#17295 = ADVANCED_FACE ( 'NONE', ( #7968 ), #9229, .T. ) ;
#17296 = EDGE_CURVE ( 'NONE', #12653, #7321, #13629, .T. ) ;
#17297 = CONICAL_SURFACE ( 'NONE', #8839, 0.7500000000000006661, 0.7853981633974511656 ) ;
#17298 = CARTESIAN_POINT ( 'NONE',  ( -25.00000000000000711, 53.00000000000000711, -38.50000000000000711 ) ) ;
#17299 = CARTESIAN_POINT ( 'NONE',  ( -9.955834737091912245, -22.82508104294696594, 31.60742750791695954 ) ) ;
#17300 = EDGE_CURVE ( 'NONE', #17811, #853, #221, .T. ) ;
#17301 = DIRECTION ( 'NONE',  ( -0.000000000000000000, -0.000000000000000000, -1.000000000000000000 ) ) ;
#17302 = CARTESIAN_POINT ( 'NONE',  ( -12.35725562635143682, -19.75228648362908501, 30.95117750791695954 ) ) ;
#17303 = DIRECTION ( 'NONE',  ( 1.000000000000000000, -0.000000000000000000, -0.000000000000000000 ) ) ;
#17304 = CARTESIAN_POINT ( 'NONE',  ( -12.64274437364858628, -19.58745947852646552, 22.42382249208304401 ) ) ;
#17305 = CARTESIAN_POINT ( 'NONE',  ( 2.500000000000001776, 65.03553390593273775, 49.64999999999999147 ) ) ;
#17306 = CARTESIAN_POINT ( 'NONE',  ( 2.066987300000001859, 63.14382582708704916, 49.30000000109246372 ) ) ;
#17307 = DIRECTION ( 'NONE',  ( 1.000000000000000000, -0.000000000000000000, -0.000000000000000000 ) ) ;
#17308 = CARTESIAN_POINT ( 'NONE',  ( -1.767766952966369765, 62.23223304703363112, 49.29999999999999716 ) ) ;
#17309 = LINE ( 'NONE', #17397, #8336 ) ;
#17310 = ORIENTED_EDGE ( 'NONE', *, *, #8459, .F. ) ;
#17311 = FILL_AREA_STYLE_COLOUR ( '', #12029 ) ;
#17312 = CARTESIAN_POINT ( 'NONE',  ( 1.461580736456473906, 62.53841926354353120, 45.85000000109246798 ) ) ;
#17313 = CARTESIAN_POINT ( 'NONE',  ( -9.999999999999994671, -24.16482700510257686, 0.3261775079169582647 ) ) ;
#17314 = CARTESIAN_POINT ( 'NONE',  ( -32.50000000000000000, 53.00000000000000711, 15.00000000000000000 ) ) ;
#17315 = CARTESIAN_POINT ( 'NONE',  ( -22.04416526290809486, -22.28918265808477628, 31.39257249208304401 ) ) ;
#17316 = ADVANCED_FACE ( 'NONE', ( #18364 ), #18267, .T. ) ;
#17317 = CARTESIAN_POINT ( 'NONE',  ( -1.461580736456473906, 65.46158073645646880, 48.05000000109247082 ) ) ;
#17318 = VERTEX_POINT ( 'NONE', #508 ) ;
#17319 = DIRECTION ( 'NONE',  ( 0.000000000000000000, -0.7893522173763268812, -0.6139406135149196864 ) ) ;
#17320 = CARTESIAN_POINT ( 'NONE',  ( -1.040834085586084257E-14, 27.62132034355962773, 54.62132034355965260 ) ) ;
#17321 = LINE ( 'NONE', #3885, #2176 ) ;
#17322 = DIRECTION ( 'NONE',  ( -0.000000000000000000, -1.000000000000000000, -0.000000000000000000 ) ) ;
#17323 = FACE_OUTER_BOUND ( 'NONE', #285, .T. ) ;
#17324 = DIRECTION ( 'NONE',  ( 0.000000000000000000, 1.224646799147353207E-16, 1.000000000000000000 ) ) ;
#17325 = CARTESIAN_POINT ( 'NONE',  ( 0.1249999999999895917, 27.16170093578836031, 58.97002704785691662 ) ) ;
#17326 = ORIENTED_EDGE ( 'NONE', *, *, #1582, .T. ) ;
#17327 = ORIENTED_EDGE ( 'NONE', *, *, #10101, .F. ) ;
#17328 = CARTESIAN_POINT ( 'NONE',  ( -13.28918265808472299, -31.04416526290805933, 38.16992750791695954 ) ) ;
#17329 = EDGE_LOOP ( 'NONE', ( #4613, #4290, #17928, #8713, #1556, #18507 ) ) ;
#17331 = EDGE_LOOP ( 'NONE', ( #4805, #286, #7120, #17773 ) ) ;
#17330 = ORIENTED_EDGE ( 'NONE', *, *, #5935, .F. ) ;
#17332 = ADVANCED_FACE ( 'NONE', ( #9136 ), #10987, .T. ) ;
#17333 = CARTESIAN_POINT ( 'NONE',  ( -11.99999999999999289, -24.16482700510258752, 0.3261775079169599856 ) ) ;
#17334 = CARTESIAN_POINT ( 'NONE',  ( -7.999999999999996447, -24.16482700510256976, 26.57617750791695954 ) ) ;
#17335 = CARTESIAN_POINT ( 'NONE',  ( 2.500000000000001776, 64.00000000000000000, 47.19999999999999574 ) ) ;
#17336 = CARTESIAN_POINT ( 'NONE',  ( 1.035533905932739751, 61.50000000000000000, 47.15000000218494591 ) ) ;
#17337 = PLANE ( 'NONE',  #11241 ) ;
#17338 = ORIENTED_EDGE ( 'NONE', *, *, #3447, .T. ) ;
#17339 = PLANE ( 'NONE',  #5362 ) ;
#17340 = ORIENTED_EDGE ( 'NONE', *, *, #861, .T. ) ;
#17341 = LINE ( 'NONE', #3910, #9392 ) ;
#17342 = ORIENTED_EDGE ( 'NONE', *, *, #17230, .F. ) ;
#17343 = CARTESIAN_POINT ( 'NONE',  ( -13.75000000000000000, -35.50000000000000000, 5.000000000000003553 ) ) ;
#17344 = ADVANCED_FACE ( 'NONE', ( #15311 ), #12165, .F. ) ;
#17345 = CARTESIAN_POINT ( 'NONE',  ( 44.99999999999998579, -1.285879139104706187E-16, -56.59999999999998010 ) ) ;
#17346 = LINE ( 'NONE', #8421, #313 ) ;
#17347 = CARTESIAN_POINT ( 'NONE',  ( 0.8561741729129460632, 66.06698729999999387, 45.30000000109247082 ) ) ;
#17348 = LINE ( 'NONE', #18918, #11588 ) ;
#17349 = CARTESIAN_POINT ( 'NONE',  ( -24.00000000000000000, 110.0000000000000000, 30.00000000000000000 ) ) ;
#17350 = CARTESIAN_POINT ( 'NONE',  ( 0.1249999999999895917, 27.33847763108499507, 59.14680374315354783 ) ) ;
#17351 = ORIENTED_EDGE ( 'NONE', *, *, #15022, .F. ) ;
#17352 = ORIENTED_EDGE ( 'NONE', *, *, #138, .T. ) ;
#17353 = CARTESIAN_POINT ( 'NONE',  ( -21.95583473709191580, -21.95952864787954084, 3.169927507916957321 ) ) ;
#17354 = LINE ( 'NONE', #2547, #6480 ) ;
#17355 = VERTEX_POINT ( 'NONE', #10696 ) ;
#17356 = COLOUR_RGB ( '', 0.31764706, 0.68627451, 0.89019608) ;
#17357 = EDGE_CURVE ( 'NONE', #2050, #2908, #4835, .T. ) ;
#17358 = CARTESIAN_POINT ( 'NONE',  ( -11.21908421996106320, -27.53959229564982181, 29.20507249208303335 ) ) ;
#17359 = DIRECTION ( 'NONE',  ( 0.000000000000000000, -1.000000000000000000, -0.000000000000000000 ) ) ;
#17360 = ORIENTED_EDGE ( 'NONE', *, *, #12281, .F. ) ;
#17361 = CARTESIAN_POINT ( 'NONE',  ( -12.92450931948790149, -21.68318583509881137, 33.14257249208304756 ) ) ;
#17362 = ORIENTED_EDGE ( 'NONE', *, *, #327, .F. ) ;
#17363 = DIRECTION ( 'NONE',  ( -0.7071067811865414665, 0.5000000000000057732, -0.5000000000000028866 ) ) ;
#17364 = ORIENTED_EDGE ( 'NONE', *, *, #13525, .F. ) ;
#17365 = CARTESIAN_POINT ( 'NONE',  ( -41.00000000000000711, 53.00000000000000711, -38.50000000000000711 ) ) ;
#17366 = LINE ( 'NONE', #2283, #11108 ) ;
#17367 = LINE ( 'NONE', #17283, #7885 ) ;
#17368 = AXIS2_PLACEMENT_3D ( 'NONE', #9353, #12397, #8656 ) ;
#17369 = CARTESIAN_POINT ( 'NONE',  ( -15.16482700510259640, -28.99999999999998224, 33.13867750791696665 ) ) ;
#17370 = PLANE ( 'NONE',  #16735 ) ;
#17371 = CARTESIAN_POINT ( 'NONE',  ( 32.50000000000000000, 52.00000000000000711, -35.00000000000000000 ) ) ;
#17372 = CARTESIAN_POINT ( 'NONE',  ( -13.75000000000000000, -35.50000000000000000, 1.500000000000000000 ) ) ;
#17373 = LINE ( 'NONE', #11673, #10500 ) ;
#17374 = ORIENTED_EDGE ( 'NONE', *, *, #16937, .F. ) ;
#17375 = AXIS2_PLACEMENT_3D ( 'NONE', #17690, #10123, #8864 ) ;
#17376 = CARTESIAN_POINT ( 'NONE',  ( -14.83517299489739649, -18.99999999999997868, 25.26367750791695599 ) ) ;
#17377 = AXIS2_PLACEMENT_3D ( 'NONE', #9812, #5601, #5707 ) ;
#17378 = CARTESIAN_POINT ( 'NONE',  ( -0.8561741729129461742, 66.06698729999999387, 48.60000000109246798 ) ) ;
#17379 = ADVANCED_FACE ( 'NONE', ( #5027 ), #3359, .F. ) ;
#17380 = EDGE_CURVE ( 'NONE', #17266, #17064, #13841, .T. ) ;
#17381 = CARTESIAN_POINT ( 'NONE',  ( -13.49542703274174116, -28.95583473709188738, 29.64257249208303691 ) ) ;
#17382 = CARTESIAN_POINT ( 'NONE',  ( -24.00000000000000000, 53.00000000000000711, 0.5000000000000004441 ) ) ;
#17383 = CARTESIAN_POINT ( 'NONE',  ( 4.592425496802577917E-16, 61.50000000000000000, 46.30000000218493739 ) ) ;
#17384 = CARTESIAN_POINT ( 'NONE',  ( -12.35725562635143682, -19.75228648362908501, 25.70117750791695599 ) ) ;
#17385 = ADVANCED_FACE ( 'NONE', ( #6594 ), #11082, .T. ) ;
#17386 = LINE ( 'NONE', #18871, #19249 ) ;
#17387 = CARTESIAN_POINT ( 'NONE',  ( -10.75228648362910100, -26.64274437364854009, 27.01367750791695954 ) ) ;
#17388 = CARTESIAN_POINT ( 'NONE',  ( -31.74999999999995737, 3.367778697655221012E-16, -2.750000000000000000 ) ) ;
#17389 = CARTESIAN_POINT ( 'NONE',  ( -40.00000000000000000, 53.00000000000000711, 30.00000000000000000 ) ) ;
#17390 = CARTESIAN_POINT ( 'NONE',  ( -2.066987300000001415, 64.00000000000000000, 45.75000000109247367 ) ) ;
#17391 = CARTESIAN_POINT ( 'NONE',  ( -41.00000000000000711, 53.00000000000000711, -44.00000000000000000 ) ) ;
#17392 = EDGE_CURVE ( 'NONE', #4412, #12326, #16692, .T. ) ;
#17393 = VECTOR ( 'NONE', #2079, 1000.000000000000000 ) ;
#17394 = VECTOR ( 'NONE', #4118, 1000.000000000000000 ) ;
#17395 = DIRECTION ( 'NONE',  ( 0.000000000000000000, -7.382983113757290994E-15, -1.000000000000000000 ) ) ;
#17396 = CARTESIAN_POINT ( 'NONE',  ( -0.8561741729129465073, 61.93301270000000613, 45.90000000109247225 ) ) ;
#17397 = CARTESIAN_POINT ( 'NONE',  ( -25.00000000000001421, 107.3545527679194436, 47.49999999999997868 ) ) ;
#17398 = ORIENTED_EDGE ( 'NONE', *, *, #19206, .F. ) ;
#17399 = EDGE_CURVE ( 'NONE', #6948, #15312, #18561, .T. ) ;
#17400 =( LENGTH_UNIT ( ) NAMED_UNIT ( * ) SI_UNIT ( .MILLI., .METRE. ) );
#17401 = CARTESIAN_POINT ( 'NONE',  ( -2.066987300000001415, 64.85617417291294373, 46.30000000109247082 ) ) ;
#17402 = CARTESIAN_POINT ( 'NONE',  ( -19.95583473709191580, -22.49542703274176603, 3.169927507916957321 ) ) ;
#17403 = CARTESIAN_POINT ( 'NONE',  ( -2.500000000000001776, 64.00000000000000000, 49.19999999999999574 ) ) ;
#17404 = CARTESIAN_POINT ( 'NONE',  ( -17.04047135212050890, -17.04416526290807710, 27.01757249208303691 ) ) ;
#17405 = VECTOR ( 'NONE', #15668, 1000.000000000000000 ) ;
#17406 = VECTOR ( 'NONE', #17030, 1000.000000000000000 ) ;
#17407 = CARTESIAN_POINT ( 'NONE',  ( 0.8561741729129472844, 61.93301270000000613, 47.60000000109246798 ) ) ;
#17408 = EDGE_CURVE ( 'NONE', #1259, #14616, #13946, .T. ) ;
#17409 = ORIENTED_EDGE ( 'NONE', *, *, #10616, .T. ) ;
#17410 = DIRECTION ( 'NONE',  ( 0.000000000000000000, 0.7071067811865454633, 0.7071067811865496822 ) ) ;
#17411 = CARTESIAN_POINT ( 'NONE',  ( 2.066987300000001415, 64.85617417291294373, 47.60000000109246798 ) ) ;
#17412 = CARTESIAN_POINT ( 'NONE',  ( -41.00000000000000711, 53.00000000000000711, 27.50000000000000000 ) ) ;
#17413 = LINE ( 'NONE', #18708, #2242 ) ;
#17414 = CARTESIAN_POINT ( 'NONE',  ( 0.000000000000000000, 64.00000000000000000, 34.99999999999999289 ) ) ;
#17415 = VECTOR ( 'NONE', #10080, 1000.000000000000000 ) ;
#17416 = EDGE_CURVE ( 'NONE', #9861, #6083, #4618, .T. ) ;
#17417 = AXIS2_PLACEMENT_3D ( 'NONE', #12268, #1785, #16586 ) ;
#17418 = ADVANCED_FACE ( 'NONE', ( #9889 ), #17264, .F. ) ;
#17419 = DIRECTION ( 'NONE',  ( -1.000000000000000000, -0.000000000000000000, -0.000000000000000000 ) ) ;
#17420 = EDGE_LOOP ( 'NONE', ( #5599, #2923 ) ) ;
#17421 = ORIENTED_EDGE ( 'NONE', *, *, #4208, .T. ) ;
#17422 = CARTESIAN_POINT ( 'NONE',  ( -8.855408670957602979, -27.35725562635137820, 2.736322492083039126 ) ) ;
#17423 = ORIENTED_EDGE ( 'NONE', *, *, #6066, .T. ) ;
#17425 = EDGE_LOOP ( 'NONE', ( #8027, #6467, #11973 ) ) ;
#17424 = ORIENTED_EDGE ( 'NONE', *, *, #1812, .F. ) ;
#17426 = CARTESIAN_POINT ( 'NONE',  ( -17.31681416490115311, -26.07549068051209318, 7.544927507916959541 ) ) ;
#17427 = EDGE_CURVE ( 'NONE', #5563, #11653, #18829, .T. ) ;
#17428 = CARTESIAN_POINT ( 'NONE',  ( -20.00369391078762860, -18.75498260482333279, 35.10742750791695244 ) ) ;
#17429 = LINE ( 'NONE', #8600, #13186 ) ;
#17430 = CARTESIAN_POINT ( 'NONE',  ( 2.500000000000001776, 65.03553390593273775, 47.35000000218494165 ) ) ;
#17431 = CARTESIAN_POINT ( 'NONE',  ( -1.040834085586084257E-14, 27.62132034355962773, 54.62132034355965260 ) ) ;
#17432 = VERTEX_POINT ( 'NONE', #5489 ) ;
#17433 = CARTESIAN_POINT ( 'NONE',  ( -9.999999999999996447, -32.50000000000001421, 3.328446124929187455 ) ) ;
#17434 = VERTEX_POINT ( 'NONE', #17350 ) ;
#17435 = LINE ( 'NONE', #3721, #626 ) ;
#17436 = ORIENTED_EDGE ( 'NONE', *, *, #7719, .T. ) ;
#17437 = CARTESIAN_POINT ( 'NONE',  ( -1.038177767593160716, 62.20757355991266024, 44.99999999999999289 ) ) ;
#17438 = CARTESIAN_POINT ( 'NONE',  ( 44.99999999999998579, 3.000000000000000000, -56.59999999999998010 ) ) ;
#17439 = DIRECTION ( 'NONE',  ( -4.081702296416016490E-16, 0.000000000000000000, -1.000000000000000000 ) ) ;
#17440 = CARTESIAN_POINT ( 'NONE',  ( 1.461580736456473684, 65.46158073645646880, 46.85000000109246798 ) ) ;
#17441 = ADVANCED_FACE ( 'NONE', ( #3732 ), #791, .F. ) ;
#17442 = CARTESIAN_POINT ( 'NONE',  ( -8.528048594804062077, -45.28611686177728046, 3.000000000000000000 ) ) ;
#17443 = DIRECTION ( 'NONE',  ( -0.000000000000000000, -1.000000000000000000, -0.000000000000000000 ) ) ;
#17444 = DIRECTION ( 'NONE',  ( -1.000000000000000000, -0.000000000000000000, -0.000000000000000000 ) ) ;
#17445 = ORIENTED_EDGE ( 'NONE', *, *, #10869, .F. ) ;
#17446 = ORIENTED_EDGE ( 'NONE', *, *, #314, .T. ) ;
#17447 = CARTESIAN_POINT ( 'NONE',  ( -19.99999999999999645, -23.83517299489738051, 39.70117750791695954 ) ) ;
#17448 = CARTESIAN_POINT ( 'NONE',  ( -2.750000000000023093, 118.0000000000000284, 37.49999999999997868 ) ) ;
#17449 = ORIENTED_EDGE ( 'NONE', *, *, #7605, .T. ) ;
#17450 = CARTESIAN_POINT ( 'NONE',  ( -15.63902057219073605, -27.04416526290807710, 9.080072492083042235 ) ) ;
#17451 = CARTESIAN_POINT ( 'NONE',  ( -5.800000000000005151, 29.74264068711930520, 56.74264068711926257 ) ) ;
#17452 =( REPRESENTATION_RELATIONSHIP ('NONE','NONE', #7912, #9996 ) REPRESENTATION_RELATIONSHIP_WITH_TRANSFORMATION ( #12359 )SHAPE_REPRESENTATION_RELATIONSHIP( ) );
#17453 = ORIENTED_EDGE ( 'NONE', *, *, #8794, .T. ) ;
#17454 = CARTESIAN_POINT ( 'NONE',  ( -12.48433729119799196, -22.35725562635139596, 38.61132249208304046 ) ) ;
#17455 = VERTEX_POINT ( 'NONE', #12741 ) ;
#17456 = CARTESIAN_POINT ( 'NONE',  ( 11.83926609531033058, -43.78611686177728046, 3.000000000000000000 ) ) ;
#17457 = VERTEX_POINT ( 'NONE', #14497 ) ;
#17458 = LINE ( 'NONE', #4030, #5323 ) ;
#17459 = CARTESIAN_POINT ( 'NONE',  ( 37.50000000000000711, -6.000000000000000000, -45.00000000000000000 ) ) ;
#17460 = LINE ( 'NONE', #17562, #11917 ) ;
#17461 = LINE ( 'NONE', #10291, #6003 ) ;
#17462 = CARTESIAN_POINT ( 'NONE',  ( -10.58745947852649927, -21.64274437364853654, 31.38867750791696309 ) ) ;
#17463 = CARTESIAN_POINT ( 'NONE',  ( -41.00000000000000711, 53.00000000000000711, -19.00000000000000000 ) ) ;
#17464 = LINE ( 'NONE', #4040, #2683 ) ;
#17465 = ORIENTED_EDGE ( 'NONE', *, *, #18972, .F. ) ;
#17466 = UNCERTAINTY_MEASURE_WITH_UNIT (LENGTH_MEASURE( 1.000000000000000082E-05 ), #7519, 'distance_accuracy_value', 'NONE');
#17467 = CARTESIAN_POINT ( 'NONE',  ( -11.21908421996106320, -27.53959229564982181, 8.205072492083036906 ) ) ;
#17468 = CARTESIAN_POINT ( 'NONE',  ( -11.64274437364854187, -30.14459132904234195, 6.451177507916957765 ) ) ;
#17469 = CARTESIAN_POINT ( 'NONE',  ( 0.8561741729129472844, 61.93301270000000613, 47.40000000109247225 ) ) ;
#17470 = CARTESIAN_POINT ( 'NONE',  ( -10.75228648362912232, -21.35725562635138530, 33.36132249208304046 ) ) ;
#17471 = VECTOR ( 'NONE', #3966, 1000.000000000000000 ) ;
#17472 = DIRECTION ( 'NONE',  ( 0.000000000000000000, -1.000000000000000000, 0.000000000000000000 ) ) ;
#17473 = VERTEX_POINT ( 'NONE', #2357 ) ;
#17474 = FACE_OUTER_BOUND ( 'NONE', #15394, .T. ) ;
#17475 = CARTESIAN_POINT ( 'NONE',  ( -11.46040770435012668, -27.78091578003887463, 27.23242750791694888 ) ) ;
#17476 = FACE_OUTER_BOUND ( 'NONE', #9408, .T. ) ;
#17477 = DIRECTION ( 'NONE',  ( 0.000000000000000000, 0.000000000000000000, 1.000000000000000000 ) ) ;
#17478 = CARTESIAN_POINT ( 'NONE',  ( 2.500000000000000000, -1.768423874527823569, 1.021000000000002794 ) ) ;
#17479 = CARTESIAN_POINT ( 'NONE',  ( -9.955834737091903364, -25.17491895705295235, 39.26757249208304046 ) ) ;
#17480 = CARTESIAN_POINT ( 'NONE',  ( -1.461580736456473906, 65.46158073645646880, 44.85000000109246798 ) ) ;
#17481 = CARTESIAN_POINT ( 'NONE',  ( -5.800448907431086099, 29.80092238452525066, 56.68308948419213777 ) ) ;
#17482 = ADVANCED_FACE ( 'NONE', ( #18737 ), #6955, .T. ) ;
#17483 = CARTESIAN_POINT ( 'NONE',  ( -2.499999999999999556, 62.96446609406726225, 48.55000000218494449 ) ) ;
#17484 = CARTESIAN_POINT ( 'NONE',  ( -1.265664690411616068E-16, 66.06698730000000808, 44.75000000109247367 ) ) ;
#17485 = ADVANCED_FACE ( 'NONE', ( #3831 ), #2048, .T. ) ;
#17486 = CARTESIAN_POINT ( 'NONE',  ( 2.500000000000000000, 2.357898499370431722, -2.818925648462311528E-15 ) ) ;
#17487 = AXIS2_PLACEMENT_3D ( 'NONE', #3387, #10730, #6433 ) ;
#17488 = ORIENTED_EDGE ( 'NONE', *, *, #8212, .T. ) ;
#17489 = EDGE_CURVE ( 'NONE', #15813, #677, #879, .T. ) ;
#17490 = CARTESIAN_POINT ( 'NONE',  ( 2.066987300000001415, 64.85617417291294373, 45.20000000109248361 ) ) ;
#17491 = CARTESIAN_POINT ( 'NONE',  ( -17.64274437364855430, -28.24771351637087236, 7.326177507916957765 ) ) ;
#17492 = DIRECTION ( 'NONE',  ( 0.000000000000000000, 0.000000000000000000, 1.000000000000000000 ) ) ;
#17493 = EDGE_CURVE ( 'NONE', #8707, #4048, #15829, .T. ) ;
#17494 = CARTESIAN_POINT ( 'NONE',  ( -11.64274437364859693, -17.85540867095757989, 38.17382249208303335 ) ) ;
#17495 = VECTOR ( 'NONE', #4182, 1000.000000000000000 ) ;
#17496 = CARTESIAN_POINT ( 'NONE',  ( 2.066987300000002303, 63.14382582708705627, 47.70000000109247651 ) ) ;
#17497 = CARTESIAN_POINT ( 'NONE',  ( -18.78091578003889595, -27.53959229564985023, 7.544927507916957765 ) ) ;
#17498 = CIRCLE ( 'NONE', #6565, 1.500000000000001332 ) ;
#17499 = CARTESIAN_POINT ( 'NONE',  ( -1.767766952966369765, 62.23223304703363112, 45.40000000218494591 ) ) ;
#17500 = VECTOR ( 'NONE', #4406, 1000.000000000000000 ) ;
#17501 = CARTESIAN_POINT ( 'NONE',  ( -0.8561741729129461742, 66.06698730000000808, 47.00000000109247367 ) ) ;
#17502 = FACE_OUTER_BOUND ( 'NONE', #18712, .T. ) ;
#17503 =( BOUNDED_SURFACE ( )  B_SPLINE_SURFACE ( 1, 2, ( 
 ( #9079, #15066, #162, #2904, #6148, #12108, #18105, #7916, #15354, #4788, #3586, #12602, #1829, #5072, #15453, #14075, #8012, #13978, #1933, #12408, #16931, #18502, #4972, #6243, #5161, #13879, #7809, #10836, #12502, #647, #16831, #9272, #17120, #3392, #455, #11124, #3303, #18307, #9559, #10929, #6441, #10737, #9467, #3684, #9363, #18406, #3493, #257, #2020, #9653, #13781, #11027, #550, #6637, #6536, #18594, #17029, #15552, #2121, #4876, #8105, #1732, #15258, #7712, #13678, #12209, #18210, #16733, #360, #6347, #12312, #741, #11496, #16028, #14351, #2588, #5257, #17396, #6814, #2489, #10027, #11399, #4169, #9836, #3870, #5633, #9752, #1120, #18881, #11209, #11595, #5351, #8477, #7002, #5538, #19060, #17216, #8206, #17592, #3783, #17484 ),
 ( #5444, #15925, #4062, #15833, #11314, #2396, #3969, #8381, #6719, #926, #15743, #2305, #6909, #18969, #17308, #9927, #12881, #8569, #14454, #15644, #14548, #1028, #12970, #7099, #12691, #13064, #2214, #14172, #18693, #8289, #14261, #832, #12780, #18778, #13168, #11990, #1621, #10225, #13463, #4465, #3075, #16412, #2976, #4362, #1417, #5926, #7487, #13365, #14644, #13559, #2882, #16212, #19260, #1519, #9055, #5832, #17685, #6121, #11795, #16317, #140, #11693, #7295, #17983, #19357, #8860, #19163, #17892, #12088, #17788, #10319, #14845, #8664, #7394, #18084, #2780, #45, #8957, #13261, #6030, #16118, #15042, #4559, #10416, #4265, #11895, #14946, #10517, #8758, #1213, #16513, #5734, #7593, #10120, #2688, #7193, #14747, #1323, #623, #16810, #3473 ) ),
 .UNSPECIFIED., .F., .F., .F. ) 
 B_SPLINE_SURFACE_WITH_KNOTS ( ( 2, 2 ),
 ( 3, 2, 2, 2, 2, 2, 2, 2, 2, 2, 2, 2, 2, 2, 2, 2, 2, 2, 2, 2, 2, 2, 2, 2, 2, 2, 2, 2, 2, 2, 2, 2, 2, 2, 2, 2, 2, 2, 2, 2, 2, 2, 2, 2, 2, 2, 2, 2, 2, 2, 3 ),
 ( 0.000000000000000000, 1.000000000000000000 ),
 ( 0.000000000000000000, 0.01785714285714285615, 0.03571428571428571230, 0.05357142857142856845, 0.07142857142857142461, 0.08928571428571428770, 0.1071428571428571369, 0.1250000000000000000, 0.1428571428571428492, 0.1607142857142857262, 0.1785714285714285754, 0.1964285714285714246, 0.2142857142857142738, 0.2321428571428571508, 0.2500000000000000000, 0.2678571428571428492, 0.2857142857142856984, 0.3035714285714285476, 0.3214285714285714524, 0.3392857142857143016, 0.3571428571428571508, 0.3750000000000000000, 0.3928571428571428492, 0.4107142857142856984, 0.4285714285714285476, 0.4464285714285714524, 0.4642857142857143016, 0.4821428571428571508, 0.5000000000000000000, 0.5178571428571429047, 0.5357142857142856984, 0.5535714285714286031, 0.5714285714285713969, 0.5892857142857143016, 0.6071428571428570953, 0.6250000000000000000, 0.6428571428571429047, 0.6607142857142856984, 0.6785714285714286031, 0.6964285714285713969, 0.7142857142857143016, 0.7321428571428570953, 0.7500000000000000000, 0.7678571428571429047, 0.7857142857142856984, 0.8035714285714286031, 0.8214285714285713969, 0.8392857142857143016, 0.8571428571428570953, 0.8750000000000000000, 0.8928571428571429047 ),
 .UNSPECIFIED. ) 
 GEOMETRIC_REPRESENTATION_ITEM ( )  RATIONAL_B_SPLINE_SURFACE ( (
 ( 1.000000000000000000, 0.9238795325112867385, 1.000000000000000000, 0.9238795325112867385, 1.000000000000000000, 0.9238795325112867385, 1.000000000000000000, 0.9238795325112867385, 1.000000000000000000, 0.9238795325112867385, 1.000000000000000000, 0.9238795325112867385, 1.000000000000000000, 0.9238795325112867385, 1.000000000000000000, 0.9238795325112867385, 1.000000000000000000, 0.9238795325112867385, 1.000000000000000000, 0.9238795325112867385, 1.000000000000000000, 0.9238795325112867385, 1.000000000000000000, 0.9238795325112867385, 1.000000000000000000, 0.9238795325112867385, 1.000000000000000000, 0.9238795325112867385, 1.000000000000000000, 0.9238795325112867385, 1.000000000000000000, 0.9238795325112867385, 1.000000000000000000, 0.9238795325112867385, 1.000000000000000000, 0.9238795325112867385, 1.000000000000000000, 0.9238795325112867385, 1.000000000000000000, 0.9238795325112867385, 1.000000000000000000, 0.9238795325112867385, 1.000000000000000000, 0.9238795325112867385, 1.000000000000000000, 0.9238795325112867385, 1.000000000000000000, 0.9238795325112867385, 1.000000000000000000, 0.9238795325112867385, 1.000000000000000000, 0.9238795325112867385, 1.000000000000000000, 0.9238795325112867385, 1.000000000000000000, 0.9238795325112867385, 1.000000000000000000, 0.9238795325112867385, 1.000000000000000000, 0.9238795325112867385, 1.000000000000000000, 0.9238795325112867385, 1.000000000000000000, 0.9238795325112867385, 1.000000000000000000, 0.9238795325112867385, 1.000000000000000000, 0.9238795325112867385, 1.000000000000000000, 0.9238795325112867385, 1.000000000000000000, 0.9238795325112867385, 1.000000000000000000, 0.9238795325112867385, 1.000000000000000000, 0.9238795325112867385, 1.000000000000000000, 0.9238795325112867385, 1.000000000000000000, 0.9238795325112867385, 1.000000000000000000, 0.9238795325112867385, 1.000000000000000000, 0.9238795325112867385, 1.000000000000000000, 0.9238795325112867385, 1.000000000000000000, 0.9238795325112867385, 1.000000000000000000, 0.9238795325112867385, 1.000000000000000000, 0.9238795325112867385, 1.000000000000000000, 0.9238795325112867385, 1.000000000000000000, 0.9238795325112867385, 1.000000000000000000, 0.9238795325112867385, 1.000000000000000000, 0.9238795325112867385, 1.000000000000000000),
 ( 1.000000000000000000, 0.9238795325112867385, 1.000000000000000000, 0.9238795325112867385, 1.000000000000000000, 0.9238795325112867385, 1.000000000000000000, 0.9238795325112867385, 1.000000000000000000, 0.9238795325112867385, 1.000000000000000000, 0.9238795325112867385, 1.000000000000000000, 0.9238795325112867385, 1.000000000000000000, 0.9238795325112867385, 1.000000000000000000, 0.9238795325112867385, 1.000000000000000000, 0.9238795325112867385, 1.000000000000000000, 0.9238795325112867385, 1.000000000000000000, 0.9238795325112867385, 1.000000000000000000, 0.9238795325112867385, 1.000000000000000000, 0.9238795325112867385, 1.000000000000000000, 0.9238795325112867385, 1.000000000000000000, 0.9238795325112867385, 1.000000000000000000, 0.9238795325112867385, 1.000000000000000000, 0.9238795325112867385, 1.000000000000000000, 0.9238795325112867385, 1.000000000000000000, 0.9238795325112867385, 1.000000000000000000, 0.9238795325112867385, 1.000000000000000000, 0.9238795325112867385, 1.000000000000000000, 0.9238795325112867385, 1.000000000000000000, 0.9238795325112867385, 1.000000000000000000, 0.9238795325112867385, 1.000000000000000000, 0.9238795325112867385, 1.000000000000000000, 0.9238795325112867385, 1.000000000000000000, 0.9238795325112867385, 1.000000000000000000, 0.9238795325112867385, 1.000000000000000000, 0.9238795325112867385, 1.000000000000000000, 0.9238795325112867385, 1.000000000000000000, 0.9238795325112867385, 1.000000000000000000, 0.9238795325112867385, 1.000000000000000000, 0.9238795325112867385, 1.000000000000000000, 0.9238795325112867385, 1.000000000000000000, 0.9238795325112867385, 1.000000000000000000, 0.9238795325112867385, 1.000000000000000000, 0.9238795325112867385, 1.000000000000000000, 0.9238795325112867385, 1.000000000000000000, 0.9238795325112867385, 1.000000000000000000, 0.9238795325112867385, 1.000000000000000000, 0.9238795325112867385, 1.000000000000000000, 0.9238795325112867385, 1.000000000000000000, 0.9238795325112867385, 1.000000000000000000, 0.9238795325112867385, 1.000000000000000000, 0.9238795325112867385, 1.000000000000000000, 0.9238795325112867385, 1.000000000000000000, 0.9238795325112867385, 1.000000000000000000, 0.9238795325112867385, 1.000000000000000000, 0.9238795325112867385, 1.000000000000000000) ) ) 
 REPRESENTATION_ITEM ( '' )  SURFACE ( )  );
#17504 = PLANE ( 'NONE',  #9130 ) ;
#17505 = DIRECTION ( 'NONE',  ( 0.000000000000000000, 0.000000000000000000, -1.000000000000000000 ) ) ;
#17506 = EDGE_CURVE ( 'NONE', #1372, #1647, #12832, .T. ) ;
#17507 = VECTOR ( 'NONE', #4521, 1000.000000000000000 ) ;
#17508 = CARTESIAN_POINT ( 'NONE',  ( -1.040834085586084257E-14, 23.37867965644034030, 50.37867965644033319 ) ) ;
#17509 = ORIENTED_EDGE ( 'NONE', *, *, #11511, .T. ) ;
#17510 = ORIENTED_EDGE ( 'NONE', *, *, #6867, .F. ) ;
#17511 = CARTESIAN_POINT ( 'NONE',  ( -18.35725562635138886, -30.14459132904237393, 4.048822492083038682 ) ) ;
#17512 = VECTOR ( 'NONE', #12154, 1000.000000000000000 ) ;
#17513 = PRESENTATION_STYLE_ASSIGNMENT (( #2517 ) ) ;
#17514 = ORIENTED_EDGE ( 'NONE', *, *, #876, .F. ) ;
#17516 = ORIENTED_EDGE ( 'NONE', *, *, #15896, .T. ) ;
#17515 = VERTEX_POINT ( 'NONE', #3642 ) ;
#17517 = CARTESIAN_POINT ( 'NONE',  ( -12.04416526290807887, -24.96867458239596260, 5.794927507916960430 ) ) ;
#17518 = CARTESIAN_POINT ( 'NONE',  ( -20.24501739517664234, -29.00369391078761439, 33.79492750791695244 ) ) ;
#17519 = VECTOR ( 'NONE', #10808, 1000.000000000000000 ) ;
#17520 = PLANE ( 'NONE',  #17282 ) ;
#17521 = CARTESIAN_POINT ( 'NONE',  ( -1.461580736456473906, 65.46158073645646880, 48.65000000109247225 ) ) ;
#17522 = CARTESIAN_POINT ( 'NONE',  ( 8.000000000000000000, 68.00000000000000000, 45.00000000000000000 ) ) ;
#17523 = ORIENTED_EDGE ( 'NONE', *, *, #545, .F. ) ;
#17524 = PLANE ( 'NONE',  #5661 ) ;
#17525 = ORIENTED_EDGE ( 'NONE', *, *, #18416, .T. ) ;
#17526 = EDGE_CURVE ( 'NONE', #6374, #6170, #5303, .T. ) ;
#17527 = EDGE_CURVE ( 'NONE', #5763, #14286, #11262, .T. ) ;
#17528 = LINE ( 'NONE', #12732, #10004 ) ;
#17529 = AXIS2_PLACEMENT_3D ( 'NONE', #12451, #18448, #5018 ) ;
#17530 = ORIENTED_EDGE ( 'NONE', *, *, #9591, .T. ) ;
#17531 = CARTESIAN_POINT ( 'NONE',  ( -24.00000000000000711, 110.0000000000000000, -44.00000000000000000 ) ) ;
#17532 = DIRECTION ( 'NONE',  ( -0.7071067811865437980, 0.5000000000000043299, -0.5000000000000008882 ) ) ;
#17533 = CARTESIAN_POINT ( 'NONE',  ( 4.012830983233651061, 32.52836399182262994, 53.60336399182268252 ) ) ;
#17534 = EDGE_CURVE ( 'NONE', #16247, #11044, #15699, .T. ) ;
#17535 = CIRCLE ( 'NONE', #18787, 1.500000000000001332 ) ;
#17536 = CARTESIAN_POINT ( 'NONE',  ( 1.461580736456473906, 62.53841926354353120, 45.05000000109246372 ) ) ;
#17537 = PLANE ( 'NONE',  #10020 ) ;
#17538 = PLANE ( 'NONE',  #14894 ) ;
#17539 = COLOUR_RGB ( '', 0.09019608, 0.27058824, 0.51372549) ;
#17540 = DIRECTION ( 'NONE',  ( 0.000000000000000000, 0.000000000000000000, 1.000000000000000000 ) ) ;
#17541 = ORIENTED_EDGE ( 'NONE', *, *, #5368, .T. ) ;
#17543 = ORIENTED_EDGE ( 'NONE', *, *, #10599, .F. ) ;
#17542 = ORIENTED_EDGE ( 'NONE', *, *, #6997, .F. ) ;
#17544 = CARTESIAN_POINT ( 'NONE',  ( -11.35725562635144925, -18.02023567606020293, -0.5488224920830435671 ) ) ;
#17545 = DIRECTION ( 'NONE',  ( 0.000000000000000000, -1.000000000000000000, 0.000000000000000000 ) ) ;
#17546 = VECTOR ( 'NONE', #6119, 1000.000000000000000 ) ;
#17547 = ORIENTED_EDGE ( 'NONE', *, *, #1479, .F. ) ;
#17548 = CARTESIAN_POINT ( 'NONE',  ( -11.21908421996106320, -27.53959229564982181, 39.70507249208304046 ) ) ;
#17549 = CARTESIAN_POINT ( 'NONE',  ( 2.749999999999981792, 118.0000000000000284, 37.49999999999997868 ) ) ;
#17550 = EDGE_CURVE ( 'NONE', #12614, #16356, #5810, .T. ) ;
#17551 = EDGE_CURVE ( 'NONE', #19093, #17940, #7144, .T. ) ;
#17552 = EDGE_LOOP ( 'NONE', ( #5101, #16851, #7250, #9087 ) ) ;
#17553 = CARTESIAN_POINT ( 'NONE',  ( -13.35725562635141195, -26.51566270880198672, 39.92382249208304756 ) ) ;
#17554 = CARTESIAN_POINT ( 'NONE',  ( 1.767766952966369987, 65.76776695296638309, 48.89999999999999858 ) ) ;
#17555 = ORIENTED_EDGE ( 'NONE', *, *, #13869, .F. ) ;
#17556 = VECTOR ( 'NONE', #11067, 1000.000000000000000 ) ;
#17557 = PLANE ( 'NONE',  #609 ) ;
#17558 = PRODUCT_DEFINITION_SHAPE ( 'NONE', 'NONE',  #19396 ) ;
#17559 = ORIENTED_EDGE ( 'NONE', *, *, #6743, .F. ) ;
#17560 = CARTESIAN_POINT ( 'NONE',  ( -41.00000000000000711, 53.00000000000000711, -6.000000000000001776 ) ) ;
#17561 = LINE ( 'NONE', #8268, #12377 ) ;
#17562 = CARTESIAN_POINT ( 'NONE',  ( -24.00000000000000000, 110.0000000000000000, 30.00000000000000000 ) ) ;
#17563 = VECTOR ( 'NONE', #2185, 1000.000000000000000 ) ;
#17564 = PRODUCT_CONTEXT ( 'NONE', #5081, 'mechanical' ) ;
#17565 = CARTESIAN_POINT ( 'NONE',  ( 8.000000000000003553, -25.00000000000000711, 1.500000000000000000 ) ) ;
#17566 = AXIS2_PLACEMENT_3D ( 'NONE', #6370, #6740, #7939 ) ;
#17567 = CARTESIAN_POINT ( 'NONE',  ( -18.53959229564986799, -20.21908421996107563, 29.85742750791695599 ) ) ;
#17568 = CARTESIAN_POINT ( 'NONE',  ( -1.485306817036799787, -17.18313764714974923, -16.36466261444977377 ) ) ;
#17569 = PRODUCT_RELATED_PRODUCT_CATEGORY ( 'part', '', ( #12997 ) ) ;
#17570 = CARTESIAN_POINT ( 'NONE',  ( -11.21908421996108629, -20.46040770435011069, 4.919927507916955989 ) ) ;
#17571 = VECTOR ( 'NONE', #2230, 1000.000000000000000 ) ;
#17572 = CARTESIAN_POINT ( 'NONE',  ( 1.300000000000000044, 1.478016689125442484, -1.626303258728256651E-15 ) ) ;
#17573 = EDGE_LOOP ( 'NONE', ( #12862, #1948 ) ) ;
#17574 = CARTESIAN_POINT ( 'NONE',  ( -19.99999999999999645, -24.16482700510261949, 10.17382249208304046 ) ) ;
#17575 = VECTOR ( 'NONE', #3985, 1000.000000000000000 ) ;
#17576 = CARTESIAN_POINT ( 'NONE',  ( -20.24501739517664234, -29.00369391078761439, 2.294927507916956433 ) ) ;
#17577 = ADVANCED_FACE ( 'NONE', ( #9005 ), #4561, .T. ) ;
#17578 = CARTESIAN_POINT ( 'NONE',  ( 1.461580736456473684, 65.46158073645646880, 46.85000000109246798 ) ) ;
#17579 = CARTESIAN_POINT ( 'NONE',  ( -17.95583473709190869, -24.96867458239598037, 4.705072492083043123 ) ) ;
#17580 = AXIS2_PLACEMENT_3D ( 'NONE', #780, #3912, #8247 ) ;
#17581 = CYLINDRICAL_SURFACE ( 'NONE', #6892, 6.000000000000000888 ) ;
#17582 = ORIENTED_EDGE ( 'NONE', *, *, #16981, .T. ) ;
#17583 = CARTESIAN_POINT ( 'NONE',  ( -24.00000000000000711, 53.00000000000000711, -5.000000000000000888 ) ) ;
#17584 = CARTESIAN_POINT ( 'NONE',  ( -9.999999999999994671, -24.16482700510257686, 31.82617750791696309 ) ) ;
#17585 = CARTESIAN_POINT ( 'NONE',  ( -44.99999999999998579, 6.000000000000000000, -53.50000000000000000 ) ) ;
#17586 = CARTESIAN_POINT ( 'NONE',  ( -32.50000000000000000, 53.00000000000000711, -35.00000000000000000 ) ) ;
#17587 = CARTESIAN_POINT ( 'NONE',  ( -2.500000000000006661, 65.03553390593272354, 46.85000000218494165 ) ) ;
#17588 = CARTESIAN_POINT ( 'NONE',  ( -17.64274437364858983, -19.75228648362910633, 37.29882249208303335 ) ) ;
#17589 = CARTESIAN_POINT ( 'NONE',  ( -2.500000000000001776, 64.00000000000000000, 46.79999999999999716 ) ) ;
#17590 = LINE ( 'NONE', #14450, #17187 ) ;
#17591 = CARTESIAN_POINT ( 'NONE',  ( 5.799999999999984723, 29.74264068711924835, 56.74264068711931230 ) ) ;
#17592 = CARTESIAN_POINT ( 'NONE',  ( -1.461580736456473906, 65.46158073645646880, 44.85000000109246798 ) ) ;
#17593 = LINE ( 'NONE', #13262, #2381 ) ;
#17594 = CIRCLE ( 'NONE', #11630, 4.250000000000000000 ) ;
#17595 = ORIENTED_EDGE ( 'NONE', *, *, #17939, .F. ) ;
#17596 = SURFACE_STYLE_FILL_AREA ( #1327 ) ;
#17597 = CARTESIAN_POINT ( 'NONE',  ( -12.35725562635143682, -19.75228648362908501, 9.951177507916959541 ) ) ;
#17598 = CARTESIAN_POINT ( 'NONE',  ( -19.99999999999999645, -23.83517299489738051, 8.201177507916957765 ) ) ;
#17599 = FACE_OUTER_BOUND ( 'NONE', #7322, .T. ) ;
#17600 = CARTESIAN_POINT ( 'NONE',  ( -18.35725562635138886, -30.14459132904237393, 35.54882249208304046 ) ) ;
#17601 = CARTESIAN_POINT ( 'NONE',  ( 0.8561741729129472844, 61.93301270000000613, 48.40000000109247225 ) ) ;
#17602 = CARTESIAN_POINT ( 'NONE',  ( -14.83517299489738761, -20.99999999999997513, 35.76367750791695954 ) ) ;
#17603 = CARTESIAN_POINT ( 'NONE',  ( -14.99999999999999645, 47.00000000000000711, 23.99999999999997868 ) ) ;
#17604 = DIRECTION ( 'NONE',  ( 0.000000000000000000, 0.000000000000000000, 1.000000000000000000 ) ) ;
#17605 = CARTESIAN_POINT ( 'NONE',  ( -3.155775640247338920, -38.39960408384397539, 3.000000000000000000 ) ) ;
#17606 = LINE ( 'NONE', #15849, #15912 ) ;
#17607 = DIRECTION ( 'NONE',  ( 0.000000000000000000, -1.000000000000000000, 0.000000000000000000 ) ) ;
#17608 = CARTESIAN_POINT ( 'NONE',  ( 2.066987300000001415, 64.85617417291294373, 47.00000000109246656 ) ) ;
#17609 = LINE ( 'NONE', #14370, #1918 ) ;
#17610 = DIRECTION ( 'NONE',  ( 0.000000000000000000, 0.7071067811865492381, -0.7071067811865456854 ) ) ;
#17611 = VERTEX_POINT ( 'NONE', #13515 ) ;
#17612 = ORIENTED_EDGE ( 'NONE', *, *, #12432, .F. ) ;
#17613 = CARTESIAN_POINT ( 'NONE',  ( -21.95583473709191580, -21.95952864787954084, 39.91992750791695954 ) ) ;
#17614 = ORIENTED_EDGE ( 'NONE', *, *, #14769, .T. ) ;
#17615 = CARTESIAN_POINT ( 'NONE',  ( -1.035533905932738641, 66.50000000000000000, 47.44999999999998863 ) ) ;
#17617 = ORIENTED_EDGE ( 'NONE', *, *, #8210, .T. ) ;
#17616 = ORIENTED_EDGE ( 'NONE', *, *, #5345, .T. ) ;
#17618 = CARTESIAN_POINT ( 'NONE',  ( -16.64274437364858272, -21.48433729119797420, 42.54882249208304756 ) ) ;
#17619 = CARTESIAN_POINT ( 'NONE',  ( -17.04047135212043784, -30.95583473709190159, 33.35742750791695244 ) ) ;
#17620 = PLANE ( 'NONE',  #67 ) ;
#17621 = CARTESIAN_POINT ( 'NONE',  ( -2.066987300000001415, 64.00000000000000000, 48.75000000109246656 ) ) ;
#17622 = DIRECTION ( 'NONE',  ( 0.000000000000000000, 0.000000000000000000, 1.000000000000000000 ) ) ;
#17623 = EDGE_LOOP ( 'NONE', ( #10891, #9802, #12755, #552 ) ) ;
#17624 = EDGE_CURVE ( 'NONE', #11781, #1447, #4311, .T. ) ;
#17625 = ADVANCED_FACE ( 'NONE', ( #13309 ), #1565, .F. ) ;
#17626 =( BOUNDED_CURVE ( )  B_SPLINE_CURVE ( 2, ( #2921, #14587, #14790, #1358, #19299, #13102, #5868, #13398, #13205 ),
 .UNSPECIFIED., .F., .F. ) 
 B_SPLINE_CURVE_WITH_KNOTS ( ( 3, 2, 2, 2, 3 ),
 ( 0.5000000000000001110, 0.5178571428571430157, 0.5357142857142858094, 0.5535714285714286031, 0.5714285714285713969 ),
 .UNSPECIFIED. ) 
 CURVE ( )  GEOMETRIC_REPRESENTATION_ITEM ( )  RATIONAL_B_SPLINE_CURVE ( ( 0.9999999999999995559, 0.9238795325112871826, 1.000000000000000000, 0.9238795325112867385, 1.000000000000000000, 0.9238795325112867385, 1.000000000000000000, 0.9238795325112867385, 1.000000000000000000 ) ) 
 REPRESENTATION_ITEM ( '' )  );
#17627 = CARTESIAN_POINT ( 'NONE',  ( -1.767766952966369765, 62.23223304703363112, 46.09999999999999432 ) ) ;
#17628 = EDGE_LOOP ( 'NONE', ( #8945, #13518, #17543, #12805 ) ) ;
#17629 = ORIENTED_EDGE ( 'NONE', *, *, #1106, .T. ) ;
#17630 = DIRECTION ( 'NONE',  ( 0.000000000000000000, 0.000000000000000000, -1.000000000000000000 ) ) ;
#17631 = CYLINDRICAL_SURFACE ( 'NONE', #18757, 2.500000000000001776 ) ;
#17632 = DIRECTION ( 'NONE',  ( 0.7071067811865463515, -0.5000000000000023315, 0.4999999999999994449 ) ) ;
#17633 = CARTESIAN_POINT ( 'NONE',  ( 2.066987300000001415, 64.00000000000000000, 49.35000000109246798 ) ) ;
#17634 = CARTESIAN_POINT ( 'NONE',  ( -40.00000000000000711, 53.00000000000000711, -11.50000000000000000 ) ) ;
#17635 = CARTESIAN_POINT ( 'NONE',  ( -41.00000000000000711, 110.0000000000000000, -24.49999999999999289 ) ) ;
#17636 = CYLINDRICAL_SURFACE ( 'NONE', #178, 1.500000000000001332 ) ;
#17637 = ORIENTED_EDGE ( 'NONE', *, *, #7072, .T. ) ;
#17639 = VERTEX_POINT ( 'NONE', #19113 ) ;
#17638 = VERTEX_POINT ( 'NONE', #14895 ) ;
#17640 = CARTESIAN_POINT ( 'NONE',  ( -9.754982604823348780, -18.99630608921234654, 4.919927507916955989 ) ) ;
#17641 = FACE_OUTER_BOUND ( 'NONE', #12783, .T. ) ;
#17642 = VERTEX_POINT ( 'NONE', #8906 ) ;
#17643 = EDGE_CURVE ( 'NONE', #17922, #9572, #12675, .T. ) ;
#17644 = ORIENTED_EDGE ( 'NONE', *, *, #12510, .T. ) ;
#17645 = CARTESIAN_POINT ( 'NONE',  ( -18.04416526290808775, -23.36097942780924441, 5.142572492083044011 ) ) ;
#17646 = EDGE_CURVE ( 'NONE', #9711, #2938, #18662, .T. ) ;
#17647 = ADVANCED_FACE ( 'NONE', ( #11646 ), #16069, .T. ) ;
#17648 = FACE_OUTER_BOUND ( 'NONE', #13395, .T. ) ;
#17649 = VERTEX_POINT ( 'NONE', #1271 ) ;
#17650 = CARTESIAN_POINT ( 'NONE',  ( -11.95583473709191047, -23.36097942780921954, 5.357427507916959541 ) ) ;
#17651 = DIRECTION ( 'NONE',  ( 0.9863224920830413467, 5.275954983314436132E-15, 0.1648270051026190230 ) ) ;
#17652 = VERTEX_POINT ( 'NONE', #16367 ) ;
#17653 = DIRECTION ( 'NONE',  ( 0.000000000000000000, 1.000000000000000000, -0.000000000000000000 ) ) ;
#17654 = ORIENTED_EDGE ( 'NONE', *, *, #17506, .T. ) ;
#17655 = LINE ( 'NONE', #13133, #10656 ) ;
#17656 = CARTESIAN_POINT ( 'NONE',  ( -40.00000000000000000, 53.00000000000000711, -45.00000000000000000 ) ) ;
#17657 = CARTESIAN_POINT ( 'NONE',  ( 32.50000000000000000, 47.00000000000000711, 15.00000000000000000 ) ) ;
#17658 = DIRECTION ( 'NONE',  ( 0.000000000000000000, 0.000000000000000000, 1.000000000000000000 ) ) ;
#17659 = CARTESIAN_POINT ( 'NONE',  ( -7.499999999999994671, -26.00000000000000355, 12.50000000000000000 ) ) ;
#17660 = CARTESIAN_POINT ( 'NONE',  ( -18.78091578003889950, -27.53959229564985378, 23.29492750791695954 ) ) ;
#17661 = AXIS2_PLACEMENT_3D ( 'NONE', #43, #14844, #19259 ) ;
#17662 = LINE ( 'NONE', #14721, #4245 ) ;
#17663 = CARTESIAN_POINT ( 'NONE',  ( -18.78091578003889950, -27.53959229564985378, 2.294927507916958209 ) ) ;
#17664 = DIRECTION ( 'NONE',  ( -1.000000000000000000, 0.000000000000000000, -0.000000000000000000 ) ) ;
#17665 = ADVANCED_FACE ( 'NONE', ( #94 ), #5875, .T. ) ;
#17666 = ORIENTED_EDGE ( 'NONE', *, *, #17950, .T. ) ;
#17667 = CARTESIAN_POINT ( 'NONE',  ( -7.955834737091903364, -25.71081734191518464, 39.26757249208304756 ) ) ;
#17668 = CARTESIAN_POINT ( 'NONE',  ( -18.64274437364853654, -29.97976432393976509, 7.326177507916955989 ) ) ;
#17669 = CARTESIAN_POINT ( 'NONE',  ( -1.265664690411616068E-16, 66.06698730000000808, 46.15000000109247225 ) ) ;
#17670 = EDGE_CURVE ( 'NONE', #7750, #18471, #17837, .T. ) ;
#17671 = CARTESIAN_POINT ( 'NONE',  ( -19.41254052147350961, -21.64274437364857562, 42.11132249208304046 ) ) ;
#17672 = DIRECTION ( 'NONE',  ( 1.000000000000000000, 0.000000000000000000, 0.000000000000000000 ) ) ;
#17673 = VERTEX_POINT ( 'NONE', #4411 ) ;
#17674 = VECTOR ( 'NONE', #12772, 1000.000000000000000 ) ;
#17675 = DIRECTION ( 'NONE',  ( -1.000000000000000000, 0.000000000000000000, -0.000000000000000000 ) ) ;
#17676 = DIRECTION ( 'NONE',  ( -0.000000000000000000, 0.000000000000000000, -1.000000000000000000 ) ) ;
#17677 = FACE_OUTER_BOUND ( 'NONE', #13658, .T. ) ;
#17678 = DIRECTION ( 'NONE',  ( 0.000000000000000000, 0.000000000000000000, -1.000000000000000000 ) ) ;
#17679 = DIRECTION ( 'NONE',  ( -1.000000000000000000, -0.000000000000000000, -0.000000000000000000 ) ) ;
#17680 = CARTESIAN_POINT ( 'NONE',  ( -18.53959229564983247, -27.78091578003891016, 35.76757249208303335 ) ) ;
#17681 = CARTESIAN_POINT ( 'NONE',  ( -1.035533905932738641, 66.50000000000000000, 48.24999999999999289 ) ) ;
#17682 = CARTESIAN_POINT ( 'NONE',  ( -1.265664690411616068E-16, 66.06698730000000808, 46.35000000109246798 ) ) ;
#17683 = EDGE_CURVE ( 'NONE', #15895, #3842, #1369, .T. ) ;
#17684 = DIRECTION ( 'NONE',  ( 1.000000000000000000, 0.000000000000000000, 0.000000000000000000 ) ) ;
#17685 = CARTESIAN_POINT ( 'NONE',  ( 2.500000000000001776, 64.00000000000000000, 47.19999999999999574 ) ) ;
#17686 = CARTESIAN_POINT ( 'NONE',  ( -40.00000000000000000, 53.00000000000000711, 30.00000000000000000 ) ) ;
#17687 = PRODUCT_DEFINITION_FORMATION_WITH_SPECIFIED_SOURCE ( 'ANY', '', #16315, .NOT_KNOWN. ) ;
#17688 = AXIS2_PLACEMENT_3D ( 'NONE', #16804, #1905, #7889 ) ;
#17689 = ORIENTED_EDGE ( 'NONE', *, *, #18170, .T. ) ;
#17690 = CARTESIAN_POINT ( 'NONE',  ( 0.000000000000000000, 0.000000000000000000, 0.000000000000000000 ) ) ;
#17691 = DIRECTION ( 'NONE',  ( 0.7071067811865537900, 0.4999999999999972800, -0.4999999999999940603 ) ) ;
#17692 = CARTESIAN_POINT ( 'NONE',  ( -18.53959229564986799, -20.21908421996107563, 3.607427507916956877 ) ) ;
#17693 = CARTESIAN_POINT ( 'NONE',  ( -2.500000000000001776, 65.03553390593273775, 47.65000000218494591 ) ) ;
#17694 = CARTESIAN_POINT ( 'NONE',  ( -15.16482700510263371, -18.99999999999997868, 11.48632249208304046 ) ) ;
#17695 = CARTESIAN_POINT ( 'NONE',  ( 1.461580736456473684, 65.46158073645646880, 47.85000000109246798 ) ) ;
#17696 = CARTESIAN_POINT ( 'NONE',  ( -9.955834737091912245, -22.82508104294696594, 0.1074275079169582509 ) ) ;
#17697 = VECTOR ( 'NONE', #13607, 1000.000000000000000 ) ;
#17698 = CARTESIAN_POINT ( 'NONE',  ( -41.00000000000000711, 110.0000000000000000, -37.50000000000000711 ) ) ;
#17699 = DIRECTION ( 'NONE',  ( -0.7071067811865312525, 8.659560562355131306E-17, -0.7071067811865637820 ) ) ;
#17700 = AXIS2_PLACEMENT_3D ( 'NONE', #13289, #19387, #5862 ) ;
#17701 = CARTESIAN_POINT ( 'NONE',  ( -40.00000000000000000, 53.00000000000000711, -25.50000000000000000 ) ) ;
#17702 = CARTESIAN_POINT ( 'NONE',  ( -25.00000000000000711, 53.00000000000000711, -32.00000000000000000 ) ) ;
#17703 = LINE ( 'NONE', #13187, #5379 ) ;
#17704 = CARTESIAN_POINT ( 'NONE',  ( 2.066987300000001859, 63.14382582708704916, 48.50000000109246656 ) ) ;
#17705 = DIRECTION ( 'NONE',  ( 0.000000000000000000, 0.000000000000000000, 1.000000000000000000 ) ) ;
#17706 = CARTESIAN_POINT ( 'NONE',  ( -41.00000000000000711, 110.0000000000000000, -6.000000000000001776 ) ) ;
#17707 = ORIENTED_EDGE ( 'NONE', *, *, #7438, .T. ) ;
#17708 = ORIENTED_EDGE ( 'NONE', *, *, #477, .F. ) ;
#17709 =( REPRESENTATION_RELATIONSHIP ('NONE','NONE', #7912, #8522 ) REPRESENTATION_RELATIONSHIP_WITH_TRANSFORMATION ( #5125 )SHAPE_REPRESENTATION_RELATIONSHIP( ) );
#17710 = CARTESIAN_POINT ( 'NONE',  ( -20.97976432393977575, -20.35725562635143504, 40.13867750791695954 ) ) ;
#17711 = VECTOR ( 'NONE', #13707, 1000.000000000000000 ) ;
#17712 = PRESENTATION_STYLE_ASSIGNMENT (( #1444 ) ) ;
#17713 = VECTOR ( 'NONE', #3685, 1000.000000000000000 ) ;
#17714 = CARTESIAN_POINT ( 'NONE',  ( -14.83517299489735741, -28.99999999999998224, 3.611322492083041347 ) ) ;
#17716 = ORIENTED_EDGE ( 'NONE', *, *, #5368, .F. ) ;
#17715 = VERTEX_POINT ( 'NONE', #14800 ) ;
#17717 = PRODUCT ( 'Browning Control Rotary Dial', 'Browning Control Rotary Dial', '', ( #17761 ) ) ;
#17718 = CARTESIAN_POINT ( 'NONE',  ( -11.95583473709191047, -23.36097942780921954, 0.1074275079169599995 ) ) ;
#17719 = CARTESIAN_POINT ( 'NONE',  ( -11.64274437364859693, -17.85540867095757989, 11.92382249208304046 ) ) ;
#17720 = CARTESIAN_POINT ( 'NONE',  ( -2.500000000000001776, 64.00000000000000000, 45.30000000218493739 ) ) ;
#17721 = CARTESIAN_POINT ( 'NONE',  ( 2.500000000000002220, 62.96446609406726935, 44.85000000218494165 ) ) ;
#17722 = ORIENTED_EDGE ( 'NONE', *, *, #7838, .F. ) ;
#17723 = ORIENTED_EDGE ( 'NONE', *, *, #1853, .T. ) ;
#17724 = CARTESIAN_POINT ( 'NONE',  ( 4.189607678530287593, 32.40336399182262284, 53.72836399182268252 ) ) ;
#17725 = ORIENTED_EDGE ( 'NONE', *, *, #9053, .T. ) ;
#17726 = VERTEX_POINT ( 'NONE', #2930 ) ;
#17727 = CARTESIAN_POINT ( 'NONE',  ( -25.00000000000000000, 110.0000000000000000, -18.00000000000000355 ) ) ;
#17728 = LINE ( 'NONE', #10561, #904 ) ;
#17729 = DIRECTION ( 'NONE',  ( -0.000000000000000000, -0.000000000000000000, -1.000000000000000000 ) ) ;
#17730 = VECTOR ( 'NONE', #17545, 1000.000000000000000 ) ;
#17731 = CARTESIAN_POINT ( 'NONE',  ( 0.8561741729129472844, 61.93301270000000613, 46.00000000109245946 ) ) ;
#17732 = STYLED_ITEM ( 'NONE', ( #13878 ), #16536 ) ;
#17733 = CARTESIAN_POINT ( 'NONE',  ( 0.000000000000000000, -32.00000000000000711, 1.500000000000000000 ) ) ;
#17734 = CARTESIAN_POINT ( 'NONE',  ( -37.50000000000002132, -6.000000000000000000, 44.99999999999997868 ) ) ;
#17735 = CARTESIAN_POINT ( 'NONE',  ( -50.00000000000001421, 3.000000000000000000, 59.99999999999997868 ) ) ;
#17736 = EDGE_LOOP ( 'NONE', ( #6876, #9394, #15299, #7329 ) ) ;
#17738 = ORIENTED_EDGE ( 'NONE', *, *, #4999, .T. ) ;
#17737 = VERTEX_POINT ( 'NONE', #4119 ) ;
#17739 = EDGE_CURVE ( 'NONE', #12535, #18711, #4511, .T. ) ;
#17741 = EDGE_CURVE ( 'NONE', #11533, #8015, #14989, .T. ) ;
#17740 = CARTESIAN_POINT ( 'NONE',  ( -8.855408670957631401, -20.64274437364852943, 5.138677507916955989 ) ) ;
#17742 = LINE ( 'NONE', #14806, #4608 ) ;
#17743 = ORIENTED_EDGE ( 'NONE', *, *, #5937, .F. ) ;
#17744 = ORIENTED_EDGE ( 'NONE', *, *, #4850, .F. ) ;
#17745 = CARTESIAN_POINT ( 'NONE',  ( -15.16482700510262482, -20.99999999999997513, 6.236322492083043123 ) ) ;
#17746 = ADVANCED_FACE ( 'NONE', ( #5686 ), #17636, .F. ) ;
#17747 = VECTOR ( 'NONE', #2837, 1000.000000000000000 ) ;
#17748 =( GEOMETRIC_REPRESENTATION_CONTEXT ( 3 ) GLOBAL_UNCERTAINTY_ASSIGNED_CONTEXT ( ( #6328 ) ) GLOBAL_UNIT_ASSIGNED_CONTEXT ( ( #18306, #12501, #3585 ) ) REPRESENTATION_CONTEXT ( 'NONE', 'WORKASPACE' ) );
#17749 = LINE ( 'NONE', #10277, #16903 ) ;
#17750 = DIRECTION ( 'NONE',  ( -1.000000000000000000, 0.000000000000000000, 0.000000000000000000 ) ) ;
#17751 = ORIENTED_EDGE ( 'NONE', *, *, #15468, .T. ) ;
#17752 = CARTESIAN_POINT ( 'NONE',  ( -12.92450931948788906, -26.31681416490114245, 0.9824275079169599856 ) ) ;
#17753 = EDGE_CURVE ( 'NONE', #4517, #19239, #8706, .T. ) ;
#17754 = LINE ( 'NONE', #15006, #14744 ) ;
#17755 = ORIENTED_EDGE ( 'NONE', *, *, #6960, .F. ) ;
#17756 = CARTESIAN_POINT ( 'NONE',  ( 2.500000000000000000, -2.357898499370432610, 3.252606517456513302E-15 ) ) ;
#17757 = ORIENTED_EDGE ( 'NONE', *, *, #11176, .F. ) ;
#17758 = DIRECTION ( 'NONE',  ( 0.000000000000000000, -1.000000000000000000, -0.000000000000000000 ) ) ;
#17759 = DIRECTION ( 'NONE',  ( -0.000000000000000000, 1.000000000000000000, 1.632680918566406547E-16 ) ) ;
#17760 = LINE ( 'NONE', #1685, #18827 ) ;
#17761 = PRODUCT_CONTEXT ( 'NONE', #4057, 'mechanical' ) ;
#17762 = CARTESIAN_POINT ( 'NONE',  ( -4.000000000000001776, 67.00000000000000000, 30.00000000000000000 ) ) ;
#17763 = CARTESIAN_POINT ( 'NONE',  ( -14.83517299489739649, -18.99999999999997868, 30.51367750791695954 ) ) ;
#17764 = CARTESIAN_POINT ( 'NONE',  ( -4.101219330882018177, 26.84264068711928530, 59.64264068711926825 ) ) ;
#17765 = CARTESIAN_POINT ( 'NONE',  ( -19.99999999999999645, -23.83517299489738051, 8.201177507916957765 ) ) ;
#17766 = DIRECTION ( 'NONE',  ( -0.000000000000000000, -0.000000000000000000, -1.000000000000000000 ) ) ;
#17767 = ORIENTED_EDGE ( 'NONE', *, *, #10420, .T. ) ;
#17768 = CARTESIAN_POINT ( 'NONE',  ( -13.82508104294702100, -18.95583473709188382, 1.205072492083041125 ) ) ;
#17769 = CARTESIAN_POINT ( 'NONE',  ( -18.53959229564986799, -20.21908421996107563, 40.35742750791696665 ) ) ;
#17770 = DIRECTION ( 'NONE',  ( -1.000000000000000000, -0.000000000000000000, -0.000000000000000000 ) ) ;
#17771 = CARTESIAN_POINT ( 'NONE',  ( -15.16482700510263371, -18.99999999999997868, 42.98632249208304046 ) ) ;
#17772 = LINE ( 'NONE', #7283, #645 ) ;
#17773 = ORIENTED_EDGE ( 'NONE', *, *, #13213, .F. ) ;
#17774 = DIRECTION ( 'NONE',  ( -1.048036716171419796E-14, -0.7071067811865496822, 0.7071067811865454633 ) ) ;
#17775 = ORIENTED_EDGE ( 'NONE', *, *, #2948, .T. ) ;
#17776 = LINE ( 'NONE', #8852, #10936 ) ;
#17777 = PLANE ( 'NONE',  #16430 ) ;
#17778 = LINE ( 'NONE', #4255, #634 ) ;
#17779 = FACE_OUTER_BOUND ( 'NONE', #7548, .T. ) ;
#17780 = CARTESIAN_POINT ( 'NONE',  ( 1.300000000000000044, -1.478016689125442706, 1.843143693225357538E-15 ) ) ;
#17781 = EDGE_CURVE ( 'NONE', #3523, #13384, #9489, .T. ) ;
#17782 = ADVANCED_FACE ( 'NONE', ( #4612 ), #12240, .T. ) ;
#17783 = CARTESIAN_POINT ( 'NONE',  ( -1.767766952966370209, 65.76776695296638309, 46.69999999999999574 ) ) ;
#17784 = CARTESIAN_POINT ( 'NONE',  ( -1.265664690411616068E-16, 66.06698730000000808, 47.15000000109247225 ) ) ;
#17785 = EDGE_CURVE ( 'NONE', #16789, #18739, #10957, .T. ) ;
#17786 = CARTESIAN_POINT ( 'NONE',  ( 4.189131392896553230, 26.90500129688588871, 59.57932772728319293 ) ) ;
#17787 = ADVANCED_FACE ( 'NONE', ( #6466 ), #1745, .T. ) ;
#17788 = CARTESIAN_POINT ( 'NONE',  ( 1.035533905932738197, 66.50000000000000000, 46.54999999999999716 ) ) ;
#17789 = FACE_OUTER_BOUND ( 'NONE', #18114, .T. ) ;
#17790 = ORIENTED_EDGE ( 'NONE', *, *, #423, .F. ) ;
#17791 = VECTOR ( 'NONE', #16527, 1000.000000000000000 ) ;
#17792 = SHAPE_REPRESENTATION_RELATIONSHIP ( 'NONE' , 'NONE' ,  #6533, #16479 ) ;
#17793 = CARTESIAN_POINT ( 'NONE',  ( -10.04416526290807710, -25.50457296725819489, 5.794927507916955989 ) ) ;
#17794 = CARTESIAN_POINT ( 'NONE',  ( -10.75228648362910100, -26.64274437364854009, 11.26367750791695777 ) ) ;
#17795 = CARTESIAN_POINT ( 'NONE',  ( -1.767766952966369765, 62.23223304703363112, 48.60000000218494165 ) ) ;
#17796 = CARTESIAN_POINT ( 'NONE',  ( -9.955834737091903364, -25.17491895705294880, 2.517572492083040903 ) ) ;
#17797 = CARTESIAN_POINT ( 'NONE',  ( 0.04165538583019195301, 33.84386001800125143, 52.64078660347674798 ) ) ;
#17798 = EDGE_CURVE ( 'NONE', #8432, #14106, #1760, .T. ) ;
#17799 = CARTESIAN_POINT ( 'NONE',  ( -12.64274437364855252, -28.41254052147347053, 6.451177507916959541 ) ) ;
#17800 = EDGE_CURVE ( 'NONE', #12743, #9436, #12138, .T. ) ;
#17801 = CARTESIAN_POINT ( 'NONE',  ( -10.58745947852649927, -21.64274437364853654, 10.38867750791695777 ) ) ;
#17802 = LINE ( 'NONE', #16224, #13178 ) ;
#17803 = CARTESIAN_POINT ( 'NONE',  ( 1.300000000000000044, 0.000000000000000000, 0.000000000000000000 ) ) ;
#17804 = LINE ( 'NONE', #1534, #9655 ) ;
#17805 = AXIS2_PLACEMENT_3D ( 'NONE', #9831, #11204, #735 ) ;
#17806 = DIRECTION ( 'NONE',  ( -1.000000000000000000, 0.000000000000000000, -0.000000000000000000 ) ) ;
#17807 = CARTESIAN_POINT ( 'NONE',  ( 2.066987300000001415, 64.85617417291294373, 45.40000000109247225 ) ) ;
#17808 = DIRECTION ( 'NONE',  ( 0.000000000000000000, 0.000000000000000000, 1.000000000000000000 ) ) ;
#17809 = DIRECTION ( 'NONE',  ( 0.000000000000000000, 0.000000000000000000, -1.000000000000000000 ) ) ;
#17810 = VERTEX_POINT ( 'NONE', #14000 ) ;
#17811 = VERTEX_POINT ( 'NONE', #4810 ) ;
#17812 = CARTESIAN_POINT ( 'NONE',  ( -9.020235676060250896, -20.35725562635137820, 22.86132249208304046 ) ) ;
#17813 = VECTOR ( 'NONE', #8331, 1000.000000000000000 ) ;
#17814 = DIRECTION ( 'NONE',  ( -1.000000000000000000, 2.470246229790980797E-15, -2.470246229790967386E-15 ) ) ;
#17816 = ORIENTED_EDGE ( 'NONE', *, *, #6786, .T. ) ;
#17815 = ORIENTED_EDGE ( 'NONE', *, *, #5549, .F. ) ;
#17817 = CARTESIAN_POINT ( 'NONE',  ( -12.68318583509884157, -21.92450931948787485, 20.66992750791696665 ) ) ;
#17818 = DIRECTION ( 'NONE',  ( 0.000000000000000000, 0.000000000000000000, -1.000000000000000000 ) ) ;
#17819 = CARTESIAN_POINT ( 'NONE',  ( -20.24501739517669563, -18.99630608921239627, 5.580072492083037794 ) ) ;
#17820 = AXIS2_PLACEMENT_3D ( 'NONE', #12646, #2350, #18643 ) ;
#17821 = CARTESIAN_POINT ( 'NONE',  ( 1.461580736456473684, 65.46158073645646880, 49.25000000109246656 ) ) ;
#17822 = CARTESIAN_POINT ( 'NONE',  ( -1.767766952966370209, 65.76776695296638309, 46.00000000218494733 ) ) ;
#17823 = VERTEX_POINT ( 'NONE', #15190 ) ;
#17824 = EDGE_CURVE ( 'NONE', #15185, #1168, #9202, .T. ) ;
#17825 = VERTEX_POINT ( 'NONE', #18038 ) ;
#17826 = DIRECTION ( 'NONE',  ( -7.304098846218135653E-17, 0.000000000000000000, 1.000000000000000000 ) ) ;
#17827 = VERTEX_POINT ( 'NONE', #10566 ) ;
#17828 = ORIENTED_EDGE ( 'NONE', *, *, #4305, .T. ) ;
#17829 = CARTESIAN_POINT ( 'NONE',  ( -12.07460121177581236, -20.93486186128575000, -1.847635612033976164E-16 ) ) ;
#17830 = DIRECTION ( 'NONE',  ( 0.000000000000000000, 0.000000000000000000, -1.000000000000000000 ) ) ;
#17831 = AXIS2_PLACEMENT_3D ( 'NONE', #8049, #16676, #18145 ) ;
#17832 = CARTESIAN_POINT ( 'NONE',  ( -2.066987300000001415, 64.00000000000000000, 48.15000000109247225 ) ) ;
#17833 =( REPRESENTATION_RELATIONSHIP ('NONE','NONE', #7912, #2502 ) REPRESENTATION_RELATIONSHIP_WITH_TRANSFORMATION ( #6203 )SHAPE_REPRESENTATION_RELATIONSHIP( ) );
#17834 = DIRECTION ( 'NONE',  ( -0.000000000000000000, -1.000000000000000000, 0.000000000000000000 ) ) ;
#17835 = VECTOR ( 'NONE', #17363, 1000.000000000000000 ) ;
#17836 = VECTOR ( 'NONE', #12554, 1000.000000000000000 ) ;
#17837 = LINE ( 'NONE', #5777, #16445 ) ;
#17838 = VERTEX_POINT ( 'NONE', #4998 ) ;
#17840 = ORIENTED_EDGE ( 'NONE', *, *, #14178, .F. ) ;
#17839 = ORIENTED_EDGE ( 'NONE', *, *, #3264, .T. ) ;
#17841 = CARTESIAN_POINT ( 'NONE',  ( -21.99999999999999289, -23.83517299489739116, 13.45117750791695777 ) ) ;
#17842 = LINE ( 'NONE', #15289, #14298 ) ;
#17843 = ORIENTED_EDGE ( 'NONE', *, *, #11472, .T. ) ;
#17844 = CIRCLE ( 'NONE', #5322, 0.7500000000000006661 ) ;
#17845 = ORIENTED_EDGE ( 'NONE', *, *, #8762, .F. ) ;
#17846 = CARTESIAN_POINT ( 'NONE',  ( -15.96867458239599635, -21.04416526290806999, 6.017572492083043123 ) ) ;
#17847 = EDGE_CURVE ( 'NONE', #18801, #10345, #15095, .T. ) ;
#17848 = AXIS2_PLACEMENT_3D ( 'NONE', #17133, #17319, #2229 ) ;
#17849 = CARTESIAN_POINT ( 'NONE',  ( 14.99999999999998579, 73.00000000000001421, 23.99999999999997158 ) ) ;
#17850 = CARTESIAN_POINT ( 'NONE',  ( -25.00000000000000711, 53.00000000000000711, 26.50000000000000000 ) ) ;
#17851 = EDGE_CURVE ( 'NONE', #14201, #11173, #10519, .T. ) ;
#17852 = EDGE_LOOP ( 'NONE', ( #17767, #8246, #13708, #13620 ) ) ;
#17853 = CARTESIAN_POINT ( 'NONE',  ( -17.31681416490115311, -26.07549068051209318, 7.544927507916959541 ) ) ;
#17854 = VECTOR ( 'NONE', #18727, 1000.000000000000000 ) ;
#17855 = DIRECTION ( 'NONE',  ( 0.000000000000000000, 0.000000000000000000, 1.000000000000000000 ) ) ;
#17856 = ORIENTED_EDGE ( 'NONE', *, *, #16313, .F. ) ;
#17857 = LINE ( 'NONE', #16383, #11255 ) ;
#17858 = VERTEX_POINT ( 'NONE', #16560 ) ;
#17859 = LINE ( 'NONE', #15010, #15358 ) ;
#17860 = CARTESIAN_POINT ( 'NONE',  ( -19.09188309203666023, 29.56586399182277347, 56.56586399182251057 ) ) ;
#17861 = LINE ( 'NONE', #6097, #19136 ) ;
#17862 =( NAMED_UNIT ( * ) PLANE_ANGLE_UNIT ( ) SI_UNIT ( $, .RADIAN. ) );
#17863 = LINE ( 'NONE', #9322, #10972 ) ;
#17864 = VECTOR ( 'NONE', #8984, 1000.000000000000000 ) ;
#17865 = CARTESIAN_POINT ( 'NONE',  ( -15.16482700510259640, -28.99999999999998224, 38.38867750791695954 ) ) ;
#17866 = CARTESIAN_POINT ( 'NONE',  ( -50.00000000000002132, 3.000000000000000000, -60.00000000000002132 ) ) ;
#17867 = CARTESIAN_POINT ( 'NONE',  ( -19.95583473709191580, -22.49542703274176603, 8.419927507916955989 ) ) ;
#17868 = AXIS2_PLACEMENT_3D ( 'NONE', #13306, #5874, #11945 ) ;
#17869 = CYLINDRICAL_SURFACE ( 'NONE', #2389, 2.500000000000001776 ) ;
#17870 = ORIENTED_EDGE ( 'NONE', *, *, #9928, .T. ) ;
#17871 = CARTESIAN_POINT ( 'NONE',  ( -12.64274437364858628, -19.58745947852646552, 6.673822492083040459 ) ) ;
#17872 = EDGE_CURVE ( 'NONE', #15564, #18046, #1897, .T. ) ;
#17873 = VECTOR ( 'NONE', #5596, 1000.000000000000000 ) ;
#17874 = CARTESIAN_POINT ( 'NONE',  ( 1.767766952966370653, 62.23223304703363112, 48.00000000218494023 ) ) ;
#17875 = CARTESIAN_POINT ( 'NONE',  ( -13.35725562635141195, -26.51566270880198672, 8.423822492083042235 ) ) ;
#17876 = DIRECTION ( 'NONE',  ( -0.000000000000000000, 1.000000000000000000, -0.000000000000000000 ) ) ;
#17877 = VERTEX_POINT ( 'NONE', #284 ) ;
#17878 = VECTOR ( 'NONE', #14619, 1000.000000000000000 ) ;
#17879 = CARTESIAN_POINT ( 'NONE',  ( -40.00000000000000000, 53.00000000000000711, -38.50000000000000711 ) ) ;
#17880 = ORIENTED_EDGE ( 'NONE', *, *, #7464, .T. ) ;
#17881 = DIRECTION ( 'NONE',  ( 0.000000000000000000, 0.000000000000000000, -1.000000000000000000 ) ) ;
#17882 = EDGE_CURVE ( 'NONE', #16762, #4322, #9105, .T. ) ;
#17883 = DIRECTION ( 'NONE',  ( -0.000000000000000000, -1.000000000000000000, -0.000000000000000000 ) ) ;
#17884 = CARTESIAN_POINT ( 'NONE',  ( 2.500000000000002220, 62.96446609406726225, 45.54999999999999005 ) ) ;
#17885 = CIRCLE ( 'NONE', #18816, 0.7500000000000006661 ) ;
#17886 = DIRECTION ( 'NONE',  ( 0.000000000000000000, 0.000000000000000000, -1.000000000000000000 ) ) ;
#17887 = DIRECTION ( 'NONE',  ( 1.000000000000000000, 0.000000000000000000, 0.000000000000000000 ) ) ;
#17888 = CARTESIAN_POINT ( 'NONE',  ( -1.461580736456473462, 62.53841926354353120, 45.85000000109246798 ) ) ;
#17889 = VECTOR ( 'NONE', #7530, 1000.000000000000000 ) ;
#17890 = PRODUCT_DEFINITION_SHAPE ( 'NONE', 'NONE',  #12776 ) ;
#17891 = CARTESIAN_POINT ( 'NONE',  ( 0.000000000000000000, 64.00000000000000000, 49.99999999999999289 ) ) ;
#17892 = CARTESIAN_POINT ( 'NONE',  ( -1.035533905932738641, 66.50000000000000000, 46.64999999999999147 ) ) ;
#17893 = CARTESIAN_POINT ( 'NONE',  ( -41.00000000000000711, 53.00000000000000711, -5.000000000000000888 ) ) ;
#17894 = VECTOR ( 'NONE', #13334, 1000.000000000000000 ) ;
#17895 = ORIENTED_EDGE ( 'NONE', *, *, #4289, .F. ) ;
#17896 =( GEOMETRIC_REPRESENTATION_CONTEXT ( 3 ) GLOBAL_UNCERTAINTY_ASSIGNED_CONTEXT ( ( #3568 ) ) GLOBAL_UNIT_ASSIGNED_CONTEXT ( ( #7762, #306, #9968 ) ) REPRESENTATION_CONTEXT ( 'NONE', 'WORKASPACE' ) );
#17897 = CARTESIAN_POINT ( 'NONE',  ( -12.64274437364855252, -28.41254052147347053, 1.201177507916958431 ) ) ;
#17898 = ADVANCED_FACE ( 'NONE', ( #194 ), #12334, .F. ) ;
#17899 = CARTESIAN_POINT ( 'NONE',  ( -10.04416526290807710, -25.50457296725819489, 16.29492750791695954 ) ) ;
#17900 = CARTESIAN_POINT ( 'NONE',  ( -2.000850093858623779, 63.37525195204790407, 45.00000000000001421 ) ) ;
#17901 = EDGE_CURVE ( 'NONE', #4393, #11621, #5272, .T. ) ;
#17902 = CARTESIAN_POINT ( 'NONE',  ( -11.21908421996106320, -27.53959229564982181, 2.955072492083040903 ) ) ;
#17903 = CARTESIAN_POINT ( 'NONE',  ( 1.461580736456473906, 62.53841926354353120, 46.85000000109246798 ) ) ;
#17904 = CARTESIAN_POINT ( 'NONE',  ( -16.17491895705301275, -18.95583473709189803, 9.294927507916954212 ) ) ;
#17905 = CARTESIAN_POINT ( 'NONE',  ( -7.499999999999994671, -38.00000000000000000, 12.50000000000000000 ) ) ;
#17906 = CARTESIAN_POINT ( 'NONE',  ( -9.967509313853890163, -23.17922740248042857, 0.1652515419773398775 ) ) ;
#17907 = CARTESIAN_POINT ( 'NONE',  ( -41.00000000000000711, 110.0000000000000000, -32.00000000000000000 ) ) ;
#17908 = VECTOR ( 'NONE', #3300, 1000.000000000000000 ) ;
#17909 = CARTESIAN_POINT ( 'NONE',  ( -35.00000000000002132, -0.000000000000000000, -42.50000000000001421 ) ) ;
#17910 = CARTESIAN_POINT ( 'NONE',  ( 1.300000000000000044, 0.000000000000000000, 0.000000000000000000 ) ) ;
#17911 = AXIS2_PLACEMENT_3D ( 'NONE', #10704, #14010, #11343 ) ;
#17912 = DIRECTION ( 'NONE',  ( 0.000000000000000000, 0.000000000000000000, -1.000000000000000000 ) ) ;
#17913 = CARTESIAN_POINT ( 'NONE',  ( -0.8561741729129466183, 61.93301270000000613, 45.10000000109246798 ) ) ;
#17914 = DIRECTION ( 'NONE',  ( 0.000000000000000000, 1.000000000000000000, 0.000000000000000000 ) ) ;
#17915 = LINE ( 'NONE', #11713, #813 ) ;
#17916 = ORIENTED_EDGE ( 'NONE', *, *, #18600, .T. ) ;
#17917 = EDGE_LOOP ( 'NONE', ( #4158, #692, #7086, #5138 ) ) ;
#17918 = CARTESIAN_POINT ( 'NONE',  ( -17.04047135212050890, -17.04416526290807710, 16.51757249208304046 ) ) ;
#17919 = EDGE_CURVE ( 'NONE', #17455, #885, #18897, .T. ) ;
#17920 = CARTESIAN_POINT ( 'NONE',  ( 2.749999999999979128, 118.0000000000000142, 40.49999999999995737 ) ) ;
#17922 = VERTEX_POINT ( 'NONE', #12800 ) ;
#17921 = VERTEX_POINT ( 'NONE', #12900 ) ;
#17923 = CARTESIAN_POINT ( 'NONE',  ( -13.64274437364856141, -26.68048971390460622, 22.20117750791696309 ) ) ;
#17924 = DIRECTION ( 'NONE',  ( -0.000000000000000000, -1.000000000000000000, -0.000000000000000000 ) ) ;
#17925 = CARTESIAN_POINT ( 'NONE',  ( -9.996306089212408708, -18.75498260482328661, 12.14257249208303691 ) ) ;
#17926 = CARTESIAN_POINT ( 'NONE',  ( -14.99999999999999645, 73.00000000000001421, 20.99999999999998224 ) ) ;
#17927 = CARTESIAN_POINT ( 'NONE',  ( 4.592425496802577917E-16, 61.50000000000000000, 45.50000000218494733 ) ) ;
#17928 = ORIENTED_EDGE ( 'NONE', *, *, #10831, .T. ) ;
#17929 = ORIENTED_EDGE ( 'NONE', *, *, #16480, .T. ) ;
#17930 = CARTESIAN_POINT ( 'NONE',  ( 1.767766952966370653, 62.23223304703363112, 46.29999999999999716 ) ) ;
#17931 = CARTESIAN_POINT ( 'NONE',  ( -1.040834085586084257E-14, 29.74264068711925901, 56.74264068711929809 ) ) ;
#17932 = CLOSED_SHELL ( 'NONE', ( #6418, #17787, #18371, #14909, #2309, #9153, #4948, #3556, #10170, #8810, #14797, #9168, #11996, #3260, #11562, #4602, #17647, #17295, #17379, #3701, #16296, #18367, #12962, #10172, #6281, #8100, #9120 ) ) ;
#17933 = EDGE_LOOP ( 'NONE', ( #8591, #8714, #13116, #14679 ) ) ;
#17934 = DIRECTION ( 'NONE',  ( -0.000000000000000000, 1.000000000000000000, -0.000000000000000000 ) ) ;
#17935 = PLANE ( 'NONE',  #1884 ) ;
#17936 = CARTESIAN_POINT ( 'NONE',  ( 2.066987300000001415, 64.00000000000000000, 46.95000000109246940 ) ) ;
#17937 = DIRECTION ( 'NONE',  ( -1.000000000000000000, 0.000000000000000000, -0.000000000000000000 ) ) ;
#17938 = CARTESIAN_POINT ( 'NONE',  ( 32.50000000000000000, 52.00000000000000711, -35.00000000000000000 ) ) ;
#17939 = EDGE_CURVE ( 'NONE', #2362, #6663, #10631, .T. ) ;
#17940 = VERTEX_POINT ( 'NONE', #11052 ) ;
#17942 = ORIENTED_EDGE ( 'NONE', *, *, #14159, .T. ) ;
#17941 = ORIENTED_EDGE ( 'NONE', *, *, #19117, .F. ) ;
#17943 = CARTESIAN_POINT ( 'NONE',  ( -17.04047135212043784, -30.95583473709190159, 22.85742750791695599 ) ) ;
#17944 = CARTESIAN_POINT ( 'NONE',  ( -40.00000000000000000, 53.00000000000000711, 30.00000000000000000 ) ) ;
#17945 = ORIENTED_EDGE ( 'NONE', *, *, #12293, .T. ) ;
#17946 = ORIENTED_EDGE ( 'NONE', *, *, #11406, .T. ) ;
#17947 = CARTESIAN_POINT ( 'NONE',  ( -15.96867458239599635, -21.04416526290806999, 21.76757249208304756 ) ) ;
#17948 = LINE ( 'NONE', #7351, #11869 ) ;
#17949 = CARTESIAN_POINT ( 'NONE',  ( -32.50000000000000000, 47.00000000000000711, 15.00000000000000000 ) ) ;
#17950 = EDGE_CURVE ( 'NONE', #16534, #19297, #18674, .T. ) ;
#17951 = ORIENTED_EDGE ( 'NONE', *, *, #8125, .F. ) ;
#17952 = CARTESIAN_POINT ( 'NONE',  ( -12.31951028609537602, -22.64274437364854364, 5.138677507916959541 ) ) ;
#17953 = CARTESIAN_POINT ( 'NONE',  ( -2.500000000000001776, 64.00000000000000000, 47.70000000218494307 ) ) ;
#17954 = ORIENTED_EDGE ( 'NONE', *, *, #16548, .F. ) ;
#17955 = CARTESIAN_POINT ( 'NONE',  ( -41.00000000000000711, 110.0000000000000000, -18.00000000000000000 ) ) ;
#17956 = ORIENTED_EDGE ( 'NONE', *, *, #2771, .F. ) ;
#17957 = DIRECTION ( 'NONE',  ( 0.000000000000000000, 0.000000000000000000, -1.000000000000000000 ) ) ;
#17958 = DIRECTION ( 'NONE',  ( -0.7071067811865463515, 0.5000000000000024425, -0.4999999999999993339 ) ) ;
#17959 = DIRECTION ( 'NONE',  ( 2.775557561562890858E-16, 0.7071067811865454633, 0.7071067811865496822 ) ) ;
#17960 = B_SPLINE_CURVE_WITH_KNOTS ( 'NONE', 3,
 ( #7578, #13546, #3165, #125 ),
 .UNSPECIFIED., .F., .F.,
 ( 4, 4 ),
 ( 0.000000000000000000, 1.000000000000000000 ),
 .UNSPECIFIED. ) ;
#17961 = APPLICATION_PROTOCOL_DEFINITION ( 'draft international standard', 'automotive_design', 1998, #6073 ) ;
#17962 = FACE_OUTER_BOUND ( 'NONE', #6443, .T. ) ;
#17963 = CARTESIAN_POINT ( 'NONE',  ( -1.767766952966370209, 65.76776695296638309, 49.89999999999999147 ) ) ;
#17964 = LINE ( 'NONE', #16392, #3315 ) ;
#17965 = CARTESIAN_POINT ( 'NONE',  ( -19.41254052147348830, -26.35725562635142083, 13.01367750791695777 ) ) ;
#17966 = DIRECTION ( 'NONE',  ( 1.000000000000000000, -0.000000000000000000, -0.000000000000000000 ) ) ;
#17967 = ORIENTED_EDGE ( 'NONE', *, *, #7105, .T. ) ;
#17968 = CARTESIAN_POINT ( 'NONE',  ( -10.04416526290808953, -22.49542703274172695, 12.58007249208304046 ) ) ;
#17969 = CARTESIAN_POINT ( 'NONE',  ( 4.592425496802577917E-16, 61.50000000000000000, 47.90000000218494591 ) ) ;
#17970 = CARTESIAN_POINT ( 'NONE',  ( -12.31951028609536536, -25.35725562635139596, 7.986322492083044011 ) ) ;
#17971 = DIRECTION ( 'NONE',  ( 0.000000000000000000, -1.000000000000000000, 0.000000000000000000 ) ) ;
#17972 = EDGE_LOOP ( 'NONE', ( #801, #16071, #18057, #16147 ) ) ;
#17973 = CARTESIAN_POINT ( 'NONE',  ( -44.99999999999998579, 3.000000000000000000, -55.00000000000000000 ) ) ;
#17974 = ORIENTED_EDGE ( 'NONE', *, *, #18977, .F. ) ;
#17975 = CARTESIAN_POINT ( 'NONE',  ( -15.00000000000000000, 0.000000000000000000, 37.00000000000000000 ) ) ;
#17976 = CARTESIAN_POINT ( 'NONE',  ( 24.99999999999998579, 107.3545527679194436, 47.49999999999997868 ) ) ;
#17977 = CARTESIAN_POINT ( 'NONE',  ( -4.189607678530257395, 32.40336399182267257, 53.72836399182263278 ) ) ;
#17978 = LINE ( 'NONE', #336, #17546 ) ;
#17979 = PRESENTATION_LAYER_ASSIGNMENT (  '', '', ( #14850 ) ) ;
#17980 = CARTESIAN_POINT ( 'NONE',  ( -11.21337592062047328, -21.65370470877428133, 1.651559915991179248E-16 ) ) ;
#17981 = CARTESIAN_POINT ( 'NONE',  ( -2.066987300000001415, 64.85617417291294373, 45.70000000109248361 ) ) ;
#17982 = FILL_AREA_STYLE_COLOUR ( '', #17356 ) ;
#17983 = CARTESIAN_POINT ( 'NONE',  ( -2.500000000000000888, 62.96446609406726935, 46.84999999999998721 ) ) ;
#17984 = CARTESIAN_POINT ( 'NONE',  ( -25.00000000000000711, 53.00000000000000711, 6.999999999999999112 ) ) ;
#17985 = ORIENTED_EDGE ( 'NONE', *, *, #3682, .T. ) ;
#17986 = EDGE_CURVE ( 'NONE', #11055, #5967, #12713, .T. ) ;
#17987 = ADVANCED_FACE ( 'NONE', ( #18710 ), #3890, .T. ) ;
#17989 =( GEOMETRIC_REPRESENTATION_CONTEXT ( 3 ) GLOBAL_UNCERTAINTY_ASSIGNED_CONTEXT ( ( #421 ) ) GLOBAL_UNIT_ASSIGNED_CONTEXT ( ( #7921, #6155, #12117 ) ) REPRESENTATION_CONTEXT ( 'NONE', 'WORKASPACE' ) );
#17988 = DIRECTION ( 'NONE',  ( 0.000000000000000000, 0.000000000000000000, 1.000000000000000000 ) ) ;
#17990 = CARTESIAN_POINT ( 'NONE',  ( -24.00000000000000000, 53.00000000000000711, 26.50000000000000000 ) ) ;
#17991 = AXIS2_PLACEMENT_3D ( 'NONE', #1111, #16109, #2580 ) ;
#17992 = CARTESIAN_POINT ( 'NONE',  ( -19.95583473709191580, -22.49542703274176603, 8.419927507916955989 ) ) ;
#17993 = CARTESIAN_POINT ( 'NONE',  ( 2.500000000000001776, 65.03553390593273775, 48.15000000218494591 ) ) ;
#17994 = EDGE_CURVE ( 'NONE', #5786, #17434, #852, .T. ) ;
#17995 = CARTESIAN_POINT ( 'NONE',  ( -19.41254052147350961, -21.64274437364857562, 5.361322492083041347 ) ) ;
#17996 = CARTESIAN_POINT ( 'NONE',  ( 3.796994071234847710E-16, 61.93301269999999903, 45.15000000109247225 ) ) ;
#17997 = CARTESIAN_POINT ( 'NONE',  ( -17.07549068051210739, -21.68318583509881847, 40.35742750791696665 ) ) ;
#17998 = ADVANCED_FACE ( 'NONE', ( #9859 ), #15857, .F. ) ;
#17999 = DIRECTION ( 'NONE',  ( -0.000000000000000000, 0.000000000000000000, 1.000000000000000000 ) ) ;
#18000 = CARTESIAN_POINT ( 'NONE',  ( -20.04416526290808065, -25.17491895705300209, 13.23242750791695777 ) ) ;
#18001 = CARTESIAN_POINT ( 'NONE',  ( -1.040834085586084257E-14, 25.49999999999998934, 52.50000000000000711 ) ) ;
#18002 = DIRECTION ( 'NONE',  ( -1.000000000000000000, 0.000000000000000000, 0.000000000000000000 ) ) ;
#18003 = CARTESIAN_POINT ( 'NONE',  ( -31.74999999999995737, 0.000000000000000000, 0.000000000000000000 ) ) ;
#18004 = EDGE_CURVE ( 'NONE', #4631, #6552, #12534, .T. ) ;
#18005 = CARTESIAN_POINT ( 'NONE',  ( -31.74999999999995737, 0.000000000000000000, 0.000000000000000000 ) ) ;
#18006 = VECTOR ( 'NONE', #10190, 1000.000000000000000 ) ;
#18007 = CARTESIAN_POINT ( 'NONE',  ( -2.066987300000001415, 64.85617417291294373, 46.50000000109246656 ) ) ;
#18008 = CARTESIAN_POINT ( 'NONE',  ( -19.99999999999999645, 0.000000000000000000, 0.000000000000000000 ) ) ;
#18009 = EDGE_CURVE ( 'NONE', #9993, #17921, #14372, .T. ) ;
#18010 = PLANE ( 'NONE',  #18979 ) ;
#18011 = ORIENTED_EDGE ( 'NONE', *, *, #13455, .F. ) ;
#18012 = ORIENTED_EDGE ( 'NONE', *, *, #19229, .T. ) ;
#18013 = CARTESIAN_POINT ( 'NONE',  ( -7.955834737091903364, -25.71081734191518464, 18.26757249208304046 ) ) ;
#18014 = PLANE ( 'NONE',  #7532 ) ;
#18016 = EDGE_LOOP ( 'NONE', ( #7477, #11478, #18338, #5993 ) ) ;
#18015 = EDGE_LOOP ( 'NONE', ( #11816, #2570, #6870, #9808, #9126, #13783, #8264, #12261, #15402, #13203, #12902, #8235 ) ) ;
#18017 = ADVANCED_FACE ( 'NONE', ( #17236 ), #948, .T. ) ;
#18018 = CARTESIAN_POINT ( 'NONE',  ( -14.03132541760401786, -21.04416526290806289, 9.732427507916959541 ) ) ;
#18019 = CARTESIAN_POINT ( 'NONE',  ( -41.00000000000000711, 53.00000000000000711, -25.50000000000000000 ) ) ;
#18020 = CARTESIAN_POINT ( 'NONE',  ( -20.00369391078762860, -18.75498260482333279, 40.35742750791695954 ) ) ;
#18021 = AXIS2_PLACEMENT_3D ( 'NONE', #13217, #16260, #11837 ) ;
#18022 = VECTOR ( 'NONE', #464, 1000.000000000000000 ) ;
#18023 = DIRECTION ( 'NONE',  ( 0.000000000000000000, 0.7071067811865494601, -0.7071067811865456854 ) ) ;
#18024 = CARTESIAN_POINT ( 'NONE',  ( -0.8561741729129465073, 61.93301270000000613, 48.10000000109246798 ) ) ;
#18025 = VERTEX_POINT ( 'NONE', #18618 ) ;
#18026 = ORIENTED_EDGE ( 'NONE', *, *, #14270, .F. ) ;
#18027 = DIRECTION ( 'NONE',  ( 7.304098846218135653E-17, 0.000000000000000000, -1.000000000000000000 ) ) ;
#18028 = DIRECTION ( 'NONE',  ( -1.000000000000000000, 0.000000000000000000, -6.672013369141567928E-17 ) ) ;
#18029 = ORIENTED_EDGE ( 'NONE', *, *, #2116, .F. ) ;
#18030 = CARTESIAN_POINT ( 'NONE',  ( 41.99999999999997868, 6.000000000000005329, 51.99999999999997868 ) ) ;
#18031 = CARTESIAN_POINT ( 'NONE',  ( 44.99999999999997158, 6.000000000000000000, 53.50000000000000000 ) ) ;
#18032 = CARTESIAN_POINT ( 'NONE',  ( -0.8561741729129461742, 66.06698729999999387, 46.40000000109246514 ) ) ;
#18033 = ADVANCED_FACE ( 'NONE', ( #3989 ), #15947, .T. ) ;
#18034 = EDGE_CURVE ( 'NONE', #15191, #15003, #3947, .T. ) ;
#18035 = LINE ( 'NONE', #7640, #4725 ) ;
#18036 = AXIS2_PLACEMENT_3D ( 'NONE', #8782, #11921, #11194 ) ;
#18037 = VECTOR ( 'NONE', #4310, 1000.000000000000000 ) ;
#18038 = CARTESIAN_POINT ( 'NONE',  ( -24.00000000000000711, 53.00000000000000711, -37.50000000000000711 ) ) ;
#18039 = ORIENTED_EDGE ( 'NONE', *, *, #9548, .T. ) ;
#18041 = ORIENTED_EDGE ( 'NONE', *, *, #4258, .F. ) ;
#18040 = ORIENTED_EDGE ( 'NONE', *, *, #13869, .T. ) ;
#18042 = EDGE_CURVE ( 'NONE', #9683, #18948, #2141, .T. ) ;
#18043 = CARTESIAN_POINT ( 'NONE',  ( -14.83517299489740715, -16.99999999999997868, 20.01367750791695954 ) ) ;
#18044 =( BOUNDED_CURVE ( )  B_SPLINE_CURVE ( 2, ( #3109, #13498, #16743, #19292, #4496, #10552, #3011, #9188, #8988 ),
 .UNSPECIFIED., .F., .F. ) 
 B_SPLINE_CURVE_WITH_KNOTS ( ( 3, 2, 2, 2, 3 ),
 ( 0.07142857142857156338, 0.08928571428571438484, 0.1071428571428571924, 0.1250000000000000000, 0.1428571428571428215 ),
 .UNSPECIFIED. ) 
 CURVE ( )  GEOMETRIC_REPRESENTATION_ITEM ( )  RATIONAL_B_SPLINE_CURVE ( ( 0.9999999999999994449, 0.9238795325112872936, 1.000000000000000000, 0.9238795325112867385, 1.000000000000000000, 0.9238795325112867385, 1.000000000000000000, 0.9238795325112868495, 0.9999999999999998890 ) ) 
 REPRESENTATION_ITEM ( '' )  );
#18045 = DIRECTION ( 'NONE',  ( -0.1648270051026182181, 0.000000000000000000, 0.9863224920830415687 ) ) ;
#18046 = VERTEX_POINT ( 'NONE', #5184 ) ;
#18047 = ORIENTED_EDGE ( 'NONE', *, *, #3882, .T. ) ;
#18048 = CARTESIAN_POINT ( 'NONE',  ( -17.95583473709190869, -24.96867458239598037, 20.45507249208304401 ) ) ;
#18049 = LINE ( 'NONE', #13226, #18476 ) ;
#18050 = CARTESIAN_POINT ( 'NONE',  ( -2.500000000000001776, 64.00000000000000000, 46.90000000218494591 ) ) ;
#18051 = VERTEX_POINT ( 'NONE', #11145 ) ;
#18052 = CARTESIAN_POINT ( 'NONE',  ( -12.31951028609537602, -22.64274437364854364, 20.88867750791696309 ) ) ;
#18053 = AXIS2_PLACEMENT_3D ( 'NONE', #1395, #16791, #4937 ) ;
#18054 = CARTESIAN_POINT ( 'NONE',  ( -1.767766952966370209, 65.76776695296638309, 47.60000000218494165 ) ) ;
#18055 = ORIENTED_EDGE ( 'NONE', *, *, #4744, .F. ) ;
#18056 = PLANE ( 'NONE',  #4071 ) ;
#18057 = ORIENTED_EDGE ( 'NONE', *, *, #12764, .T. ) ;
#18058 = EDGE_CURVE ( 'NONE', #3796, #1874, #17140, .T. ) ;
#18059 = DIRECTION ( 'NONE',  ( 0.000000000000000000, 1.000000000000000000, 0.000000000000000000 ) ) ;
#18060 = CARTESIAN_POINT ( 'NONE',  ( -10.31147837279037738, -22.25502639194775512, -4.119453415160654225E-17 ) ) ;
#18061 = DIRECTION ( 'NONE',  ( 0.000000000000000000, -1.000000000000000000, 0.000000000000000000 ) ) ;
#18062 = CARTESIAN_POINT ( 'NONE',  ( 2.500000000000000000, 2.357898499370431722, -2.818925648462311528E-15 ) ) ;
#18063 = CARTESIAN_POINT ( 'NONE',  ( 1.767766952966369987, 65.76776695296638309, 48.20000000218494307 ) ) ;
#18064 = CARTESIAN_POINT ( 'NONE',  ( -19.99999999999999645, -23.83517299489738051, 39.70117750791695954 ) ) ;
#18065 = CYLINDRICAL_SURFACE ( 'NONE', #5150, 2.500000000000000444 ) ;
#18066 = CARTESIAN_POINT ( 'NONE',  ( -13.49542703274178379, -19.04416526290806289, 9.732427507916959541 ) ) ;
#18067 = CIRCLE ( 'NONE', #19319, 1.599999999999997202 ) ;
#18068 = DIRECTION ( 'NONE',  ( 0.000000000000000000, 0.000000000000000000, -1.000000000000000000 ) ) ;
#18069 = ORIENTED_EDGE ( 'NONE', *, *, #280, .F. ) ;
#18070 = AXIS2_PLACEMENT_3D ( 'NONE', #19279, #15065, #10341 ) ;
#18071 = CARTESIAN_POINT ( 'NONE',  ( -20.04416526290809131, -22.82508104294699791, 15.64257249208304223 ) ) ;
#18072 = PRODUCT_DEFINITION ( 'UNKNOWN', '', #7677, #6107 ) ;
#18073 = CYLINDRICAL_SURFACE ( 'NONE', #4451, 2.500000000000001776 ) ;
#18074 = CARTESIAN_POINT ( 'NONE',  ( -14.03132541760400009, -26.95583473709189448, 24.39257249208304046 ) ) ;
#18075 = CARTESIAN_POINT ( 'NONE',  ( -14.99999999999999645, 47.00000000000000711, 20.99999999999998224 ) ) ;
#18076 = ORIENTED_EDGE ( 'NONE', *, *, #12291, .F. ) ;
#18077 = LINE ( 'NONE', #10605, #9057 ) ;
#18078 = ORIENTED_EDGE ( 'NONE', *, *, #16980, .T. ) ;
#18079 = EDGE_CURVE ( 'NONE', #19125, #6660, #14194, .T. ) ;
#18080 = CARTESIAN_POINT ( 'NONE',  ( -18.78091578003889950, -27.53959229564985378, 39.04492750791695954 ) ) ;
#18081 = PLANE ( 'NONE',  #1077 ) ;
#18082 = CARTESIAN_POINT ( 'NONE',  ( -40.00000000000000711, 53.00000000000000711, 27.50000000000000000 ) ) ;
#18083 = CARTESIAN_POINT ( 'NONE',  ( -0.8561741729129466183, 61.93301270000000613, 47.50000000109246656 ) ) ;
#18084 = CARTESIAN_POINT ( 'NONE',  ( 1.767766952966370653, 62.23223304703363112, 46.29999999999999716 ) ) ;
#18085 = LINE ( 'NONE', #4856, #516 ) ;
#18086 = UNCERTAINTY_MEASURE_WITH_UNIT (LENGTH_MEASURE( 1.000000000000000082E-05 ), #12843, 'distance_accuracy_value', 'NONE');
#18087 = ORIENTED_EDGE ( 'NONE', *, *, #4258, .T. ) ;
#18088 = DIRECTION ( 'NONE',  ( 0.000000000000000000, 0.000000000000000000, 1.000000000000000000 ) ) ;
#18089 = B_SPLINE_CURVE_WITH_KNOTS ( 'NONE', 3,
 ( #90, #4604, #2924, #3120, #7433, #10461, #9101, #17829, #16553, #17980, #14794, #4405, #15090, #13603, #1364, #5972, #10367, #16455 ),
 .UNSPECIFIED., .F., .F.,
 ( 4, 2, 2, 2, 2, 2, 2, 2, 4 ),
 ( 0.000000000000000000, 0.001329345720928956512, 0.001994018581393434877, 0.002658691441857913024, 0.003988037162786874090, 0.004652710023251353105, 0.004985046453483592613, 0.005151214668599710632, 0.005317382883715828651 ),
 .UNSPECIFIED. ) ;
#18090 = CARTESIAN_POINT ( 'NONE',  ( -16.50457296725820555, -28.95583473709189448, 12.35742750791695954 ) ) ;
#18091 = CARTESIAN_POINT ( 'NONE',  ( -10.75228648362910100, -26.64274437364854009, 16.51367750791695954 ) ) ;
#18092 = CARTESIAN_POINT ( 'NONE',  ( 1.035533905932738197, 66.50000000000000000, 48.25000000218493312 ) ) ;
#18093 = CARTESIAN_POINT ( 'NONE',  ( -10.58745947852648328, -26.35725562635138530, 13.23632249208304046 ) ) ;
#18094 = CARTESIAN_POINT ( 'NONE',  ( 0.8561741729129460632, 66.06698729999999387, 45.50000000109247367 ) ) ;
#18095 = CARTESIAN_POINT ( 'NONE',  ( -15.16482700510259640, -28.99999999999998224, 1.638677507916958431 ) ) ;
#18096 = CARTESIAN_POINT ( 'NONE',  ( -44.99999999999998579, 3.000000000000000000, -55.00000000000000000 ) ) ;
#18097 = CARTESIAN_POINT ( 'NONE',  ( -16.17491895705301275, -18.95583473709189448, 25.04492750791695599 ) ) ;
#18098 = CARTESIAN_POINT ( 'NONE',  ( 37.50000000000000711, 0.000000000000000000, -45.00000000000000000 ) ) ;
#18099 = DIRECTION ( 'NONE',  ( -0.000000000000000000, -0.000000000000000000, -1.000000000000000000 ) ) ;
#18100 = EDGE_CURVE ( 'NONE', #9810, #13646, #12988, .T. ) ;
#18101 = CARTESIAN_POINT ( 'NONE',  ( -0.8561741729129461742, 66.06698729999999387, 46.40000000109246514 ) ) ;
#18102 = DIRECTION ( 'NONE',  ( -7.709882115452476934E-17, 0.000000000000000000, -1.000000000000000000 ) ) ;
#18103 = CARTESIAN_POINT ( 'NONE',  ( -2.500000000000001776, 64.00000000000000000, 49.19999999999999574 ) ) ;
#18104 = CARTESIAN_POINT ( 'NONE',  ( -1.265664690411616068E-16, 66.06698730000000808, 46.35000000109246798 ) ) ;
#18105 = CARTESIAN_POINT ( 'NONE',  ( 1.461580736456473684, 65.46158073645646880, 49.45000000109246940 ) ) ;
#18106 = DIRECTION ( 'NONE',  ( -7.709882115452476934E-17, 0.000000000000000000, -1.000000000000000000 ) ) ;
#18107 = CARTESIAN_POINT ( 'NONE',  ( 0.000000000000000000, 0.000000000000000000, 12.50000000000000000 ) ) ;
#18108 = ORIENTED_EDGE ( 'NONE', *, *, #15174, .T. ) ;
#18109 = ORIENTED_EDGE ( 'NONE', *, *, #17919, .T. ) ;
#18110 = CARTESIAN_POINT ( 'NONE',  ( -21.99999999999999289, -24.16482700510262305, 15.42382249208304046 ) ) ;
#18111 = EDGE_CURVE ( 'NONE', #11, #9239, #11813, .T. ) ;
#18112 = SHAPE_REPRESENTATION_RELATIONSHIP ( 'NONE' , 'NONE' ,  #15417, #18799 ) ;
#18113 = CARTESIAN_POINT ( 'NONE',  ( -15.16482700510263371, -18.99999999999997868, 6.236322492083041347 ) ) ;
#18115 = ORIENTED_EDGE ( 'NONE', *, *, #8565, .F. ) ;
#18114 = EDGE_LOOP ( 'NONE', ( #10653, #16973, #1510, #16233 ) ) ;
#18116 = CARTESIAN_POINT ( 'NONE',  ( -12.48433729119798130, -25.64274437364855075, 11.26367750791696132 ) ) ;
#18117 = CARTESIAN_POINT ( 'NONE',  ( -12.50000000000000000, -35.50000000000000000, 5.000000000000003553 ) ) ;
#18118 = CARTESIAN_POINT ( 'NONE',  ( -12.95952864787948755, -30.95583473709188382, 8.642572492083038682 ) ) ;
#18119 = CARTESIAN_POINT ( 'NONE',  ( 1.461580736456473906, 62.53841926354353120, 49.05000000109247082 ) ) ;
#18120 = CARTESIAN_POINT ( 'NONE',  ( 2.066987300000002303, 63.14382582708705627, 45.90000000109247225 ) ) ;
#18121 = ORIENTED_EDGE ( 'NONE', *, *, #3159, .T. ) ;
#18122 = ORIENTED_EDGE ( 'NONE', *, *, #15990, .F. ) ;
#18123 = DIRECTION ( 'NONE',  ( 0.000000000000000000, 0.000000000000000000, -1.000000000000000000 ) ) ;
#18124 = CARTESIAN_POINT ( 'NONE',  ( -40.00000000000000000, 53.00000000000000711, 30.00000000000000000 ) ) ;
#18125 = VERTEX_POINT ( 'NONE', #19377 ) ;
#18126 = CARTESIAN_POINT ( 'NONE',  ( -2.066987300000000971, 63.14382582708704916, 48.80000000109247082 ) ) ;
#18127 = CARTESIAN_POINT ( 'NONE',  ( 7.500000000000005329, -26.00000000000000000, 12.50000000000000000 ) ) ;
#18128 = EDGE_CURVE ( 'NONE', #10014, #3899, #3267, .T. ) ;
#18129 = CARTESIAN_POINT ( 'NONE',  ( -1.265664690411616068E-16, 66.06698730000000808, 46.35000000109246798 ) ) ;
#18130 = DIRECTION ( 'NONE',  ( 1.000000000000000000, -0.000000000000000000, -0.000000000000000000 ) ) ;
#18131 = AXIS2_PLACEMENT_3D ( 'NONE', #2730, #2825, #1263 ) ;
#18132 = DIRECTION ( 'NONE',  ( 0.000000000000000000, 1.000000000000000000, 0.000000000000000000 ) ) ;
#18133 = ORIENTED_EDGE ( 'NONE', *, *, #2860, .T. ) ;
#18135 = ORIENTED_EDGE ( 'NONE', *, *, #5719, .F. ) ;
#18134 = VERTEX_POINT ( 'NONE', #1343 ) ;
#18136 = CARTESIAN_POINT ( 'NONE',  ( -11.35725562635144925, -18.02023567606020293, 9.951177507916955989 ) ) ;
#18137 = VECTOR ( 'NONE', #9746, 1000.000000000000000 ) ;
#18138 =( NAMED_UNIT ( * ) PLANE_ANGLE_UNIT ( ) SI_UNIT ( $, .RADIAN. ) );
#18139 = EDGE_LOOP ( 'NONE', ( #509, #18179, #12273, #5559 ) ) ;
#18140 = ORIENTED_EDGE ( 'NONE', *, *, #18079, .F. ) ;
#18141 = CARTESIAN_POINT ( 'NONE',  ( -11.99999999999999289, -23.83517299489735564, 18.04882249208304046 ) ) ;
#18142 = CARTESIAN_POINT ( 'NONE',  ( -9.020235676060220698, -27.64274437364852588, 6.013677507916956877 ) ) ;
#18143 = EDGE_CURVE ( 'NONE', #13986, #1960, #4287, .T. ) ;
#18144 = EDGE_CURVE ( 'NONE', #2359, #5315, #17915, .T. ) ;
#18145 = DIRECTION ( 'NONE',  ( -1.000000000000000000, 0.000000000000000000, -9.251858538542970348E-17 ) ) ;
#18146 = LINE ( 'NONE', #14811, #18177 ) ;
#18147 = EDGE_LOOP ( 'NONE', ( #15291, #1890, #13596, #11551 ) ) ;
#18148 = EDGE_CURVE ( 'NONE', #1057, #4945, #19281, .T. ) ;
#18149 = CARTESIAN_POINT ( 'NONE',  ( -11.99999999999999289, -24.16482700510258752, 21.32617750791695954 ) ) ;
#18150 = DIRECTION ( 'NONE',  ( -1.156482317317871478E-16, 1.000000000000000000, 0.000000000000000000 ) ) ;
#18151 = ORIENTED_EDGE ( 'NONE', *, *, #958, .F. ) ;
#18152 = LINE ( 'NONE', #18256, #7 ) ;
#18153 = EDGE_LOOP ( 'NONE', ( #9473, #2133, #8446, #17289 ) ) ;
#18154 = DIRECTION ( 'NONE',  ( -1.156482317317871478E-16, 1.000000000000000000, 0.000000000000000000 ) ) ;
#18155 = CYLINDRICAL_SURFACE ( 'NONE', #17079, 1.249999999999999334 ) ;
#18156 = VECTOR ( 'NONE', #11112, 1000.000000000000000 ) ;
#18157 = LINE ( 'NONE', #10689, #12245 ) ;
#18158 = CONTEXT_DEPENDENT_SHAPE_REPRESENTATION ( #8087, #14579 ) ;
#18159 = VECTOR ( 'NONE', #3699, 1000.000000000000114 ) ;
#18160 = CARTESIAN_POINT ( 'NONE',  ( 4.999999999999997335, 0.000000000000000000, -2.700000000000000622 ) ) ;
#18161 = LINE ( 'NONE', #10692, #22 ) ;
#18162 =( BOUNDED_CURVE ( )  B_SPLINE_CURVE ( 2, ( #13164, #1116, #10117, #18878, #2303, #5630, #16116, #11310, #7097, #17306, #8474, #4059, #3868, #9925, #13061, #12968, #5255, #14349, #5442, #8662, #11397, #15923, #18964, #5535, #11493, #1209, #12085, #13458, #14743, #5732, #14843, #16511, #16610, #137, #1706, #8754, #8858, #1415, #19161, #2777, #7686, #14945, #6120, #1321, #7293, #18083, #11891, #2974, #15039, #16210, #13260, #4557, #17784, #4656, #10316, #19258, #10610, #7389, #1618, #13362, #8952, #9154, #5826, #11691, #13557, #11792, #3176, #16312, #17682, #16410, #11987, #19354, #15138, #10512, #4360, #7483, #4260, #5922, #17888, #4462, #10221, #17981, #10414, #2880, #3073, #1516, #41, #6028, #9052, #7590, #6221, #10907, #12385, #18382, #14047, #6417, #15435, #4951, #16806, #15236, #1999 ),
 .UNSPECIFIED., .F., .F. ) 
 B_SPLINE_CURVE_WITH_KNOTS ( ( 3, 2, 2, 2, 2, 2, 2, 2, 2, 2, 2, 2, 2, 2, 2, 2, 2, 2, 2, 2, 2, 2, 2, 2, 2, 2, 2, 2, 2, 2, 2, 2, 2, 2, 2, 2, 2, 2, 2, 2, 2, 2, 2, 2, 2, 2, 2, 2, 2, 2, 3 ),
 ( 0.000000000000000000, 0.01785714285714285615, 0.03571428571428571230, 0.05357142857142856845, 0.07142857142857142461, 0.08928571428571428770, 0.1071428571428571369, 0.1250000000000000000, 0.1428571428571428492, 0.1607142857142857262, 0.1785714285714285754, 0.1964285714285714246, 0.2142857142857142738, 0.2321428571428571508, 0.2500000000000000000, 0.2678571428571428492, 0.2857142857142856984, 0.3035714285714285476, 0.3214285714285714524, 0.3392857142857143016, 0.3571428571428571508, 0.3750000000000000000, 0.3928571428571428492, 0.4107142857142856984, 0.4285714285714285476, 0.4464285714285714524, 0.4642857142857143016, 0.4821428571428571508, 0.5000000000000000000, 0.5178571428571429047, 0.5357142857142856984, 0.5535714285714286031, 0.5714285714285713969, 0.5892857142857143016, 0.6071428571428570953, 0.6250000000000000000, 0.6428571428571429047, 0.6607142857142856984, 0.6785714285714286031, 0.6964285714285715079, 0.7142857142857143016, 0.7321428571428570953, 0.7500000000000000000, 0.7678571428571429047, 0.7857142857142856984, 0.8035714285714286031, 0.8214285714285713969, 0.8392857142857143016, 0.8571428571428570953, 0.8750000000000000000, 0.8928571428571429047 ),
 .UNSPECIFIED. ) 
 CURVE ( )  GEOMETRIC_REPRESENTATION_ITEM ( )  RATIONAL_B_SPLINE_CURVE ( ( 1.000000000000000000, 0.9238795325112867385, 1.000000000000000000, 0.9238795325112867385, 1.000000000000000000, 0.9238795325112867385, 1.000000000000000000, 0.9238795325112867385, 1.000000000000000000, 0.9238795325112867385, 1.000000000000000000, 0.9238795325112867385, 1.000000000000000000, 0.9238795325112867385, 1.000000000000000000, 0.9238795325112867385, 1.000000000000000000, 0.9238795325112867385, 1.000000000000000000, 0.9238795325112867385, 1.000000000000000000, 0.9238795325112867385, 1.000000000000000000, 0.9238795325112867385, 1.000000000000000000, 0.9238795325112867385, 1.000000000000000000, 0.9238795325112867385, 1.000000000000000000, 0.9238795325112867385, 1.000000000000000000, 0.9238795325112867385, 1.000000000000000000, 0.9238795325112867385, 1.000000000000000000, 0.9238795325112867385, 1.000000000000000000, 0.9238795325112867385, 1.000000000000000000, 0.9238795325112867385, 1.000000000000000000, 0.9238795325112867385, 1.000000000000000000, 0.9238795325112867385, 1.000000000000000000, 0.9238795325112867385, 1.000000000000000000, 0.9238795325112867385, 1.000000000000000000, 0.9238795325112867385, 1.000000000000000000, 0.9238795325112867385, 1.000000000000000000, 0.9238795325112867385, 1.000000000000000000, 0.9238795325112867385, 1.000000000000000000, 0.9238795325112867385, 1.000000000000000000, 0.9238795325112867385, 1.000000000000000000, 0.9238795325112867385, 1.000000000000000000, 0.9238795325112867385, 1.000000000000000000, 0.9238795325112867385, 1.000000000000000000, 0.9238795325112867385, 1.000000000000000000, 0.9238795325112867385, 1.000000000000000000, 0.9238795325112867385, 1.000000000000000000, 0.9238795325112867385, 1.000000000000000000, 0.9238795325112867385, 1.000000000000000000, 0.9238795325112867385, 1.000000000000000000, 0.9238795325112867385, 1.000000000000000000, 0.9238795325112867385, 1.000000000000000000, 0.9238795325112867385, 1.000000000000000000, 0.9238795325112867385, 1.000000000000000000, 0.9238795325112867385, 1.000000000000000000, 0.9238795325112867385, 1.000000000000000000, 0.9238795325112867385, 1.000000000000000000, 0.9238795325112867385, 1.000000000000000000, 0.9238795325112867385, 1.000000000000000000, 0.9238795325112867385, 1.000000000000000000, 0.9238795325112867385, 1.000000000000000000 ) ) 
 REPRESENTATION_ITEM ( '' )  );
#18163 = CARTESIAN_POINT ( 'NONE',  ( -9.955834737091912245, -22.82508104294696594, 36.85742750791696665 ) ) ;
#18164 = CARTESIAN_POINT ( 'NONE',  ( 5.799999999999985612, 29.65425233947092920, 56.47747564417436195 ) ) ;
#18165 = ORIENTED_EDGE ( 'NONE', *, *, #2088, .T. ) ;
#18166 = CARTESIAN_POINT ( 'NONE',  ( -12.64274437364855252, -28.41254052147347053, 11.70117750791695777 ) ) ;
#18167 = AXIS2_PLACEMENT_3D ( 'NONE', #16971, #18543, #12542 ) ;
#18168 = CARTESIAN_POINT ( 'NONE',  ( -44.99999999999998579, 3.000000000000000000, -55.00000000000000000 ) ) ;
#18169 = ORIENTED_EDGE ( 'NONE', *, *, #4354, .T. ) ;
#18170 = EDGE_CURVE ( 'NONE', #9366, #17827, #4087, .T. ) ;
#18171 = CARTESIAN_POINT ( 'NONE',  ( -12.35725562635140307, -28.24771351637085459, 18.92382249208304401 ) ) ;
#18172 = VECTOR ( 'NONE', #10974, 1000.000000000000000 ) ;
#18173 = CARTESIAN_POINT ( 'NONE',  ( -3.155775640247338920, -41.39960408384398249, 3.000000000000000000 ) ) ;
#18174 = CARTESIAN_POINT ( 'NONE',  ( -15.96867458239599635, -21.04416526290806999, 16.51757249208304046 ) ) ;
#18175 = LINE ( 'NONE', #4753, #10962 ) ;
#18176 = ORIENTED_EDGE ( 'NONE', *, *, #18394, .F. ) ;
#18177 = VECTOR ( 'NONE', #13418, 1000.000000000000114 ) ;
#18178 = DIRECTION ( 'NONE',  ( 1.000000000000000000, -0.000000000000000000, 0.000000000000000000 ) ) ;
#18179 = ORIENTED_EDGE ( 'NONE', *, *, #14694, .T. ) ;
#18180 = DIRECTION ( 'NONE',  ( -1.000000000000000000, 0.000000000000000000, 0.000000000000000000 ) ) ;
#18181 = DIRECTION ( 'NONE',  ( 0.000000000000000000, 0.000000000000000000, 1.000000000000000000 ) ) ;
#18182 = CARTESIAN_POINT ( 'NONE',  ( -7.499999999999994671, -26.00000000000000355, 4.500000000000000888 ) ) ;
#18183 = AXIS2_PLACEMENT_3D ( 'NONE', #12981, #2503, #14187 ) ;
#18184 = PLANE ( 'NONE',  #7833 ) ;
#18185 = CIRCLE ( 'NONE', #1908, 2.649999999999999467 ) ;
#18186 = FILL_AREA_STYLE_COLOUR ( '', #6709 ) ;
#18187 = DIRECTION ( 'NONE',  ( 0.000000000000000000, 0.000000000000000000, 1.000000000000000000 ) ) ;
#18188 = DIRECTION ( 'NONE',  ( -0.000000000000000000, -0.000000000000000000, -1.000000000000000000 ) ) ;
#18189 = AXIS2_PLACEMENT_3D ( 'NONE', #2555, #892, #17181 ) ;
#18190 = EDGE_CURVE ( 'NONE', #10448, #578, #6464, .T. ) ;
#18191 = VERTEX_POINT ( 'NONE', #16139 ) ;
#18192 = CARTESIAN_POINT ( 'NONE',  ( 0.000000000000000000, 3.000000000000000000, 0.000000000000000000 ) ) ;
#18193 = AXIS2_PLACEMENT_3D ( 'NONE', #11889, #16608, #10807 ) ;
#18194 = CARTESIAN_POINT ( 'NONE',  ( -18.78091578003889950, -27.53959229564985378, 23.29492750791695954 ) ) ;
#18195 = CARTESIAN_POINT ( 'NONE',  ( -1.767766952966370209, 65.76776695296638309, 46.00000000218494733 ) ) ;
#18196 = CARTESIAN_POINT ( 'NONE',  ( -19.95583473709190514, -25.50457296725822687, 25.70507249208304756 ) ) ;
#18197 = VECTOR ( 'NONE', #15384, 1000.000000000000000 ) ;
#18198 = LINE ( 'NONE', #13569, #10393 ) ;
#18199 = EDGE_CURVE ( 'NONE', #12504, #4615, #2709, .T. ) ;
#18200 = CARTESIAN_POINT ( 'NONE',  ( -13.49542703274178379, -19.04416526290806289, 20.23242750791696309 ) ) ;
#18201 = LINE ( 'NONE', #60, #14535 ) ;
#18202 = CARTESIAN_POINT ( 'NONE',  ( -12.64274437364855252, -28.41254052147347053, 11.70117750791695777 ) ) ;
#18203 = CARTESIAN_POINT ( 'NONE',  ( 2.500000000000001776, 64.00000000000000000, 47.19999999999999574 ) ) ;
#18204 = DIRECTION ( 'NONE',  ( 0.000000000000000000, -1.000000000000000000, 0.000000000000000000 ) ) ;
#18205 = VECTOR ( 'NONE', #7134, 1000.000000000000000 ) ;
#18206 = CARTESIAN_POINT ( 'NONE',  ( 1.461580736456473684, 65.46158073645646880, 47.05000000109247082 ) ) ;
#18207 = LINE ( 'NONE', #19277, #18483 ) ;
#18208 = CYLINDRICAL_SURFACE ( 'NONE', #10999, 2.500000000000001776 ) ;
#18209 = CARTESIAN_POINT ( 'NONE',  ( 24.99999999999999289, -6.000000000000000000, -42.49999999999999289 ) ) ;
#18210 = CARTESIAN_POINT ( 'NONE',  ( -1.461580736456473906, 65.46158073645646880, 46.45000000109246940 ) ) ;
#18211 = PLANE ( 'NONE',  #13632 ) ;
#18212 = VECTOR ( 'NONE', #10976, 1000.000000000000000 ) ;
#18214 = ORIENTED_EDGE ( 'NONE', *, *, #1361, .T. ) ;
#18213 = EDGE_CURVE ( 'NONE', #14054, #6948, #8682, .T. ) ;
#18215 = ORIENTED_EDGE ( 'NONE', *, *, #15902, .F. ) ;
#18216 = CARTESIAN_POINT ( 'NONE',  ( -8.855408670957602979, -27.35725562635137820, 13.23632249208303868 ) ) ;
#18217 = CARTESIAN_POINT ( 'NONE',  ( -9.999999999999994671, -23.83517299489734143, 12.79882249208304046 ) ) ;
#18218 = ORIENTED_EDGE ( 'NONE', *, *, #16388, .F. ) ;
#18219 = CARTESIAN_POINT ( 'NONE',  ( -11.99999999999999289, -24.16482700510258752, 10.82617750791695954 ) ) ;
#18220 = PLANE ( 'NONE',  #14259 ) ;
#18221 = CARTESIAN_POINT ( 'NONE',  ( -9.020235676060250896, -20.35725562635137820, 17.61132249208303335 ) ) ;
#18222 = CIRCLE ( 'NONE', #18846, 2.999999999999999112 ) ;
#18223 = CARTESIAN_POINT ( 'NONE',  ( -1.265664690411616068E-16, 66.06698730000000808, 49.35000000109246798 ) ) ;
#18224 = CARTESIAN_POINT ( 'NONE',  ( -1.461580736456473462, 62.53841926354353120, 46.45000000109246940 ) ) ;
#18225 = ORIENTED_EDGE ( 'NONE', *, *, #17551, .T. ) ;
#18226 = EDGE_LOOP ( 'NONE', ( #14090, #17942, #14801, #5952 ) ) ;
#18227 = AXIS2_PLACEMENT_3D ( 'NONE', #4069, #12977, #9758 ) ;
#18228 = CARTESIAN_POINT ( 'NONE',  ( -41.00000000000000711, 53.00000000000000711, 26.50000000000000000 ) ) ;
#18229 = CARTESIAN_POINT ( 'NONE',  ( -15.00000000000000000, -32.00000000000000711, 3.500000000000006661 ) ) ;
#18230 = VERTEX_POINT ( 'NONE', #16232 ) ;
#18231 = CARTESIAN_POINT ( 'NONE',  ( 0.8561741729129471734, 61.93301270000000613, 48.20000000109247651 ) ) ;
#18232 = LINE ( 'NONE', #10659, #8444 ) ;
#18233 = CARTESIAN_POINT ( 'NONE',  ( -1.461580736456473462, 62.53841926354353120, 45.85000000109246798 ) ) ;
#18234 = CARTESIAN_POINT ( 'NONE',  ( -25.00000000000000000, 53.00000000000000711, -24.49999999999999289 ) ) ;
#18235 = CARTESIAN_POINT ( 'NONE',  ( 4.592425496802577917E-16, 61.50000000000000000, 45.50000000218494733 ) ) ;
#18236 = ORIENTED_EDGE ( 'NONE', *, *, #2784, .F. ) ;
#18238 = VERTEX_POINT ( 'NONE', #16341 ) ;
#18237 = ORIENTED_EDGE ( 'NONE', *, *, #4960, .T. ) ;
#18239 = CARTESIAN_POINT ( 'NONE',  ( -22.04416526290807710, -25.71081734191525925, 18.48242750791695954 ) ) ;
#18240 = VECTOR ( 'NONE', #6524, 1000.000000000000000 ) ;
#18241 =( NAMED_UNIT ( * ) SI_UNIT ( $, .STERADIAN. ) SOLID_ANGLE_UNIT ( ) );
#18242 = EDGE_LOOP ( 'NONE', ( #305, #3212, #15232, #8502 ) ) ;
#18243 = ORIENTED_EDGE ( 'NONE', *, *, #1619, .F. ) ;
#18244 = CARTESIAN_POINT ( 'NONE',  ( -17.31681416490117087, -21.92450931948788551, 10.83007249208304223 ) ) ;
#18245 = ADVANCED_FACE ( 'NONE', ( #1439 ), #2906, .F. ) ;
#18246 = EDGE_CURVE ( 'NONE', #16414, #6946, #1758, .T. ) ;
#18247 = CARTESIAN_POINT ( 'NONE',  ( -7.999999999999996447, -24.16482700510256976, 16.07617750791695599 ) ) ;
#18248 = AXIS2_PLACEMENT_3D ( 'NONE', #19300, #14791, #14887 ) ;
#18249 = CARTESIAN_POINT ( 'NONE',  ( 2.066987300000001415, 64.00000000000000000, 47.55000000109247082 ) ) ;
#18250 = FACE_OUTER_BOUND ( 'NONE', #7624, .T. ) ;
#18251 = VERTEX_POINT ( 'NONE', #1239 ) ;
#18252 = CARTESIAN_POINT ( 'NONE',  ( -14.83517299489738761, -20.99999999999997513, 14.76367750791695954 ) ) ;
#18253 = EDGE_CURVE ( 'NONE', #1259, #17515, #13968, .T. ) ;
#18254 = FILL_AREA_STYLE_COLOUR ( '', #2519 ) ;
#18255 = ORIENTED_EDGE ( 'NONE', *, *, #16837, .T. ) ;
#18256 = CARTESIAN_POINT ( 'NONE',  ( 46.99999999999998579, 6.000000000000005329, 59.99999999999997868 ) ) ;
#18257 = VERTEX_POINT ( 'NONE', #18990 ) ;
#18258 = CARTESIAN_POINT ( 'NONE',  ( -40.00000000000000711, 53.00000000000000711, 14.50000000000000000 ) ) ;
#18259 = CARTESIAN_POINT ( 'NONE',  ( 11.00000000000000355, 1.665213485140613626E-16, -1.219500000000000028 ) ) ;
#18260 = CARTESIAN_POINT ( 'NONE',  ( -3.999999999999999112, 52.00000000000000711, 30.00000000000000000 ) ) ;
#18261 = CARTESIAN_POINT ( 'NONE',  ( 0.1249999999999895917, 31.97002704785689531, 54.16170093578840294 ) ) ;
#18262 = CARTESIAN_POINT ( 'NONE',  ( 0.000000000000000000, -0.7390083445627200209, 1.280000000000001137 ) ) ;
#18263 = DIRECTION ( 'NONE',  ( 0.000000000000000000, 0.000000000000000000, -1.000000000000000000 ) ) ;
#18264 = LINE ( 'NONE', #10783, #15988 ) ;
#18265 = CARTESIAN_POINT ( 'NONE',  ( -12.64274437364855252, -28.41254052147347053, 37.95117750791695954 ) ) ;
#18266 = EDGE_CURVE ( 'NONE', #2159, #15084, #8953, .T. ) ;
#18267 = CYLINDRICAL_SURFACE ( 'NONE', #19272, 2.500000000000001776 ) ;
#18268 = ORIENTED_EDGE ( 'NONE', *, *, #10546, .T. ) ;
#18269 = ADVANCED_FACE ( 'NONE', ( #13383 ), #5950, .T. ) ;
#18270 = CARTESIAN_POINT ( 'NONE',  ( -11.21908421996108629, -20.46040770435011069, 15.41992750791695954 ) ) ;
#18271 = ADVANCED_FACE ( 'NONE', ( #1645 ), #4680, .F. ) ;
#18272 = CARTESIAN_POINT ( 'NONE',  ( -41.00000000000000711, 53.00000000000000711, 1.500000000000001332 ) ) ;
#18273 = VERTEX_POINT ( 'NONE', #18675 ) ;
#18274 = CARTESIAN_POINT ( 'NONE',  ( -15.16482700510263371, -18.99999999999997868, 16.73632249208304401 ) ) ;
#18275 = CARTESIAN_POINT ( 'NONE',  ( -13.35725562635141195, -26.51566270880198672, 13.67382249208304401 ) ) ;
#18276 = VERTEX_POINT ( 'NONE', #12012 ) ;
#18277 = CARTESIAN_POINT ( 'NONE',  ( 3.099999999999998757, 0.000000000000000000, 0.000000000000000000 ) ) ;
#18278 = VERTEX_POINT ( 'NONE', #3098 ) ;
#18279 = CARTESIAN_POINT ( 'NONE',  ( 1.300000000000000044, 0.7390083445627193548, -1.280000000000000693 ) ) ;
#18280 = FACE_OUTER_BOUND ( 'NONE', #7125, .T. ) ;
#18281 =( BOUNDED_CURVE ( )  B_SPLINE_CURVE ( 2, ( #13195, #12019, #4492, #2715, #16537, #8687, #3006, #14671, #3105, #9086, #19189, #5756, #17714, #4292, #10249, #10743, #6447, #6250, #16740, #3308, #13687, #18314, #8110, #7724, #18113, #6355, #367, #9472, #14080, #7819, #15558, #264, #12318, #4882, #9184, #8018, #17035, #12216, #15458, #461, #13787, #12416, #10843, #3592, #9279, #15171, #13885, #6156, #16838, #3401, #9370, #4685, #15365, #2126, #18217, #3503, #4979, #18511, #1938, #10937, #1835, #10643, #18412, #7922, #16940, #12118, #2027, #13985, #555, #6542, #4794, #12509, #15266, #5078, #11036, #9563, #16646, #3211, #1739, #11022, #8099, #18401, #6810, #12775, #11117, #2208, #12685, #18771, #5344, #3866, #6530, #9648, #3581, #15739, #6434, #11306, #8377, #3775, #17304, #14068, #640, #9832, #13971, #15635, #9462, #8200, #736, #9747, #6631, #15545, #12598, #14167, #18589, #4966, #5156, #15825, #17024, #12401, #6715, #17114, #10924, #544, #9553, #2115, #8004, #17209, #3678, #2015, #12495, #18688, #16925, #5253, #18497, #15448, #2301, #5066, #11205, #8285, #14255, #827, #2392, #449, #3487, #8659, #7291, #1207, #7188, #8563, #5628, #10115, #11590, #10216, #5532, #2676, #7094, #1022, #4056, #5729, #13162, #17680, #19159, #14741, #18874, #3963, #16112, #16310, #17588, #11687, #14640, #2583, #8472, #4257, #2483, #4164, #16208, #17479, #14347, #2878, #13058, #10022, #2775, #1319, #8752, #18962, #14541, #1114, #4358, #14447, #13257, #16024, #19256, #9923, #19055 ),
 .UNSPECIFIED., .F., .F. ) 
 B_SPLINE_CURVE_WITH_KNOTS ( ( 3, 2, 2, 2, 2, 2, 2, 2, 2, 2, 2, 2, 2, 2, 2, 2, 2, 2, 2, 2, 2, 2, 2, 2, 2, 2, 2, 2, 2, 2, 2, 2, 2, 2, 2, 2, 2, 2, 2, 2, 2, 2, 2, 2, 2, 2, 2, 2, 2, 2, 2, 2, 2, 2, 2, 2, 2, 2, 2, 2, 2, 2, 2, 2, 2, 2, 2, 2, 2, 2, 2, 2, 2, 2, 2, 2, 2, 2, 2, 2, 2, 2, 2, 2, 2, 2, 2, 2, 2, 2, 2, 2, 2, 2, 2, 2, 3 ),
 ( 0.000000000000000000, 0.01041666666666666609, 0.02083333333333333218, 0.03125000000000000000, 0.04166666666666666435, 0.05208333333333333565, 0.06250000000000000000, 0.07291666666666667129, 0.08333333333333332871, 0.09375000000000000000, 0.1041666666666666713, 0.1145833333333333287, 0.1250000000000000000, 0.1354166666666666574, 0.1458333333333333426, 0.1562500000000000000, 0.1666666666666666574, 0.1770833333333333426, 0.1875000000000000000, 0.1979166666666666574, 0.2083333333333333426, 0.2187500000000000000, 0.2291666666666666574, 0.2395833333333333426, 0.2500000000000000000, 0.2604166666666666852, 0.2708333333333333148, 0.2812500000000000000, 0.2916666666666666852, 0.3020833333333333148, 0.3125000000000000000, 0.3229166666666666852, 0.3333333333333333148, 0.3437500000000000000, 0.3541666666666666852, 0.3645833333333333148, 0.3750000000000000000, 0.3854166666666666852, 0.3958333333333333148, 0.4062500000000000000, 0.4166666666666666852, 0.4270833333333333148, 0.4375000000000000000, 0.4479166666666666852, 0.4583333333333333148, 0.4687500000000000000, 0.4791666666666666852, 0.4895833333333333148, 0.5000000000000000000, 0.5104166666666666297, 0.5208333333333333703, 0.5312500000000000000, 0.5416666666666666297, 0.5520833333333333703, 0.5625000000000000000, 0.5729166666666666297, 0.5833333333333333703, 0.5937500000000000000, 0.6041666666666666297, 0.6145833333333333703, 0.6250000000000000000, 0.6354166666666666297, 0.6458333333333333703, 0.6562500000000000000, 0.6666666666666666297, 0.6770833333333333703, 0.6875000000000000000, 0.6979166666666666297, 0.7083333333333333703, 0.7187500000000000000, 0.7291666666666666297, 0.7395833333333333703, 0.7500000000000000000, 0.7604166666666666297, 0.7708333333333333703, 0.7812500000000000000, 0.7916666666666666297, 0.8020833333333333703, 0.8125000000000000000, 0.8229166666666666297, 0.8333333333333333703, 0.8437500000000000000, 0.8541666666666666297, 0.8645833333333333703, 0.8750000000000000000, 0.8854166666666666297, 0.8958333333333333703, 0.9062500000000000000, 0.9166666666666666297, 0.9270833333333333703, 0.9375000000000000000, 0.9479166666666666297, 0.9583333333333333703, 0.9687500000000000000, 0.9791666666666666297, 0.9895833333333333703, 1.000000000000000000 ),
 .UNSPECIFIED. ) 
 CURVE ( )  GEOMETRIC_REPRESENTATION_ITEM ( )  RATIONAL_B_SPLINE_CURVE ( ( 1.000000000000000000, 0.9659258262890683122, 1.000000000000000000, 0.9659258262890683122, 1.000000000000000000, 0.9659258262890683122, 1.000000000000000000, 0.9659258262890683122, 1.000000000000000000, 0.9659258262890683122, 1.000000000000000000, 0.9659258262890683122, 1.000000000000000000, 0.9659258262890683122, 1.000000000000000000, 0.9659258262890683122, 1.000000000000000000, 0.9659258262890683122, 1.000000000000000000, 0.9659258262890683122, 1.000000000000000000, 0.9659258262890683122, 1.000000000000000000, 0.9659258262890683122, 1.000000000000000000, 0.9659258262890683122, 1.000000000000000000, 0.9659258262890683122, 1.000000000000000000, 0.9659258262890683122, 1.000000000000000000, 0.9659258262890683122, 1.000000000000000000, 0.9659258262890683122, 1.000000000000000000, 0.9659258262890683122, 1.000000000000000000, 0.9659258262890683122, 1.000000000000000000, 0.9659258262890683122, 1.000000000000000000, 0.9659258262890683122, 1.000000000000000000, 0.9659258262890683122, 1.000000000000000000, 0.9659258262890683122, 1.000000000000000000, 0.9659258262890683122, 1.000000000000000000, 0.9659258262890683122, 1.000000000000000000, 0.9659258262890683122, 1.000000000000000000, 0.9659258262890683122, 1.000000000000000000, 0.9659258262890683122, 1.000000000000000000, 0.9659258262890683122, 1.000000000000000000, 0.9659258262890683122, 1.000000000000000000, 0.9659258262890683122, 1.000000000000000000, 0.9659258262890683122, 1.000000000000000000, 0.9659258262890683122, 1.000000000000000000, 0.9659258262890683122, 1.000000000000000000, 0.9659258262890683122, 1.000000000000000000, 0.9659258262890683122, 1.000000000000000000, 0.9659258262890683122, 1.000000000000000000, 0.9659258262890683122, 1.000000000000000000, 0.9659258262890683122, 1.000000000000000000, 0.9659258262890683122, 1.000000000000000000, 0.9659258262890683122, 1.000000000000000000, 0.9659258262890683122, 1.000000000000000000, 0.9659258262890683122, 1.000000000000000000, 0.9659258262890683122, 1.000000000000000000, 0.9659258262890683122, 1.000000000000000000, 0.9659258262890683122, 1.000000000000000000, 0.9659258262890683122, 1.000000000000000000, 0.9659258262890683122, 1.000000000000000000, 0.9659258262890683122, 1.000000000000000000, 0.9659258262890683122, 1.000000000000000000, 0.9659258262890683122, 1.000000000000000000, 0.9659258262890683122, 1.000000000000000000, 0.9659258262890683122, 1.000000000000000000, 0.9659258262890683122, 1.000000000000000000, 0.9659258262890683122, 1.000000000000000000, 0.9659258262890683122, 1.000000000000000000, 0.9659258262890683122, 1.000000000000000000, 0.9659258262890683122, 1.000000000000000000, 0.9659258262890683122, 1.000000000000000000, 0.9659258262890683122, 1.000000000000000000, 0.9659258262890683122, 1.000000000000000000, 0.9659258262890683122, 1.000000000000000000, 0.9659258262890683122, 1.000000000000000000, 0.9659258262890683122, 1.000000000000000000, 0.9659258262890683122, 1.000000000000000000, 0.9659258262890683122, 1.000000000000000000, 0.9659258262890683122, 1.000000000000000000, 0.9659258262890683122, 1.000000000000000000, 0.9659258262890683122, 1.000000000000000000, 0.9659258262890683122, 1.000000000000000000, 0.9659258262890683122, 1.000000000000000000, 0.9659258262890683122, 1.000000000000000000, 0.9659258262890683122, 1.000000000000000000, 0.9659258262890683122, 1.000000000000000000, 0.9659258262890683122, 1.000000000000000000, 0.9659258262890683122, 1.000000000000000000, 0.9659258262890683122, 1.000000000000000000, 0.9659258262890683122, 1.000000000000000000, 0.9659258262890683122, 1.000000000000000000, 0.9659258262890683122, 1.000000000000000000, 0.9659258262890683122, 1.000000000000000000, 0.9659258262890683122, 1.000000000000000000, 0.9659258262890683122, 1.000000000000000000, 0.9659258262890683122, 1.000000000000000000, 0.9659258262890683122, 1.000000000000000000, 0.9659258262890683122, 1.000000000000000000, 0.9659258262890683122, 1.000000000000000000, 0.9659258262890683122, 1.000000000000000000, 0.9659258262890683122, 1.000000000000000000, 0.9659258262890683122, 1.000000000000000000, 0.9659258262890683122, 1.000000000000000000, 0.9659258262890683122, 1.000000000000000000, 0.9659258262890683122, 1.000000000000000000, 0.9659258262890683122, 1.000000000000000000, 0.9659258262890683122, 1.000000000000000000, 0.9659258262890683122, 1.000000000000000000 ) ) 
 REPRESENTATION_ITEM ( '' )  );
#18282 = FACE_OUTER_BOUND ( 'NONE', #5190, .T. ) ;
#18283 = CARTESIAN_POINT ( 'NONE',  ( -1.040834085586084257E-14, 27.62132034355962773, 54.62132034355965260 ) ) ;
#18284 = EDGE_CURVE ( 'NONE', #9708, #17726, #8037, .T. ) ;
#18285 = ADVANCED_FACE ( 'NONE', ( #2104 ), #5241, .F. ) ;
#18286 = CARTESIAN_POINT ( 'NONE',  ( -50.00000000000002132, 118.0000000000000142, 40.49999999999997868 ) ) ;
#18288 = LINE ( 'NONE', #16614, #6624 ) ;
#18287 = B_SPLINE_CURVE_WITH_KNOTS ( 'NONE', 3,
 ( #11980, #13251, #16401, #8746, #7285, #13647, #16504, #11882, #10307, #19250, #13550, #5818, #10407, #129, #16302, #2872, #13354, #4650, #1509, #14835, #6115, #3067, #9046, #4454 ),
 .UNSPECIFIED., .F., .F.,
 ( 4, 2, 2, 2, 2, 2, 2, 2, 2, 2, 2, 4 ),
 ( 0.005317382883715828651, 0.005430869497434138646, 0.005544356111152449508, 0.005771329338589079039, 0.006225275793462339835, 0.007133168703208861428, 0.008041061612955383020, 0.008948954522701904613, 0.009856847432448426205, 0.01076474034219494780, 0.01167263325194146766, 0.01258052616168798925 ),
 .UNSPECIFIED. ) ;
#18289 = LINE ( 'NONE', #240, #5828 ) ;
#18290 = ORIENTED_EDGE ( 'NONE', *, *, #15601, .T. ) ;
#18291 = ADVANCED_FACE ( 'NONE', ( #13682 ), #724, .T. ) ;
#18292 = CARTESIAN_POINT ( 'NONE',  ( 0.000000000000000000, 3.000000000000000000, 0.000000000000000000 ) ) ;
#18293 = CARTESIAN_POINT ( 'NONE',  ( -17.64274437364855430, -28.24771351637087236, 12.57617750791695777 ) ) ;
#18294 = CARTESIAN_POINT ( 'NONE',  ( -1.767766952966369765, 62.23223304703363112, 44.60000000218494165 ) ) ;
#18295 = CARTESIAN_POINT ( 'NONE',  ( -17.64274437364858983, -19.75228648362910633, 16.29882249208304046 ) ) ;
#18296 = DIRECTION ( 'NONE',  ( 0.000000000000000000, 0.000000000000000000, -1.000000000000000000 ) ) ;
#18297 = CARTESIAN_POINT ( 'NONE',  ( -16.50457296725820555, -28.95583473709189448, 12.35742750791695954 ) ) ;
#18298 = LINE ( 'NONE', #1821, #6723 ) ;
#18299 = CARTESIAN_POINT ( 'NONE',  ( -10.04416526290807710, -25.50457296725819489, 16.29492750791695954 ) ) ;
#18300 = FACE_OUTER_BOUND ( 'NONE', #14211, .T. ) ;
#18301 = CARTESIAN_POINT ( 'NONE',  ( -1.767766952966370209, 65.76776695296638309, 45.89999999999999858 ) ) ;
#18302 = EDGE_CURVE ( 'NONE', #11839, #17089, #6151, .T. ) ;
#18303 = CARTESIAN_POINT ( 'NONE',  ( -1.461580736456473462, 62.53841926354353120, 48.25000000109246656 ) ) ;
#18304 = CARTESIAN_POINT ( 'NONE',  ( 5.199999999999996625, 0.000000000000000000, -2.700000000000000622 ) ) ;
#18305 = CARTESIAN_POINT ( 'NONE',  ( -41.00000000000000711, 110.0000000000000000, 27.50000000000000000 ) ) ;
#18306 =( LENGTH_UNIT ( ) NAMED_UNIT ( * ) SI_UNIT ( .MILLI., .METRE. ) );
#18307 = CARTESIAN_POINT ( 'NONE',  ( 0.8561741729129460632, 66.06698729999999387, 47.90000000109247225 ) ) ;
#18308 = LINE ( 'NONE', #3393, #18037 ) ;
#18309 = MECHANICAL_DESIGN_GEOMETRIC_PRESENTATION_REPRESENTATION (  '', ( #4520 ), #16092 ) ;
#18310 = ORIENTED_EDGE ( 'NONE', *, *, #16915, .T. ) ;
#18311 = ORIENTED_EDGE ( 'NONE', *, *, #6285, .T. ) ;
#18312 = CARTESIAN_POINT ( 'NONE',  ( -9.996306089212408708, -18.75498260482328661, 27.89257249208303691 ) ) ;
#18313 = PRESENTATION_STYLE_ASSIGNMENT (( #3210 ) ) ;
#18314 = CARTESIAN_POINT ( 'NONE',  ( -18.78091578003892792, -20.46040770435013556, 5.580072492083041347 ) ) ;
#18315 = ORIENTED_EDGE ( 'NONE', *, *, #15836, .T. ) ;
#18316 = CARTESIAN_POINT ( 'NONE',  ( -12.48433729119798130, -25.64274437364855075, 27.01367750791695954 ) ) ;
#18317 = LINE ( 'NONE', #11038, #15534 ) ;
#18318 = CARTESIAN_POINT ( 'NONE',  ( -20.97976432393974022, -27.64274437364858628, 20.23632249208303691 ) ) ;
#18319 = CARTESIAN_POINT ( 'NONE',  ( -1.461580736456473906, 65.46158073645646880, 46.25000000109247367 ) ) ;
#18320 = CARTESIAN_POINT ( 'NONE',  ( 2.066987300000001415, 64.00000000000000000, 45.15000000109247225 ) ) ;
#18321 = ORIENTED_EDGE ( 'NONE', *, *, #8403, .T. ) ;
#18322 = ORIENTED_EDGE ( 'NONE', *, *, #6184, .T. ) ;
#18323 = MECHANICAL_DESIGN_GEOMETRIC_PRESENTATION_REPRESENTATION (  '', ( #10457 ), #12668 ) ;
#18324 = LINE ( 'NONE', #4894, #10350 ) ;
#18325 = DIRECTION ( 'NONE',  ( -0.7071067811865486830, -0.5000000000000005551, 0.4999999999999978351 ) ) ;
#18326 = AXIS2_PLACEMENT_3D ( 'NONE', #17976, #13254, #8853 ) ;
#18327 = ORIENTED_EDGE ( 'NONE', *, *, #9041, .F. ) ;
#18328 = DIRECTION ( 'NONE',  ( -0.000000000000000000, -0.000000000000000000, -1.000000000000000000 ) ) ;
#18329 = CARTESIAN_POINT ( 'NONE',  ( -1.530808498934192803E-16, 66.50000000000000000, 49.99999999999999289 ) ) ;
#18330 = DIRECTION ( 'NONE',  ( 9.251858538542970348E-17, 0.000000000000000000, -1.000000000000000000 ) ) ;
#18331 = CARTESIAN_POINT ( 'NONE',  ( -41.00000000000000711, 53.00000000000000711, -19.00000000000000000 ) ) ;
#18332 = CARTESIAN_POINT ( 'NONE',  ( 7.500000000000005329, -38.00000000000000000, 4.500000000000000888 ) ) ;
#18333 = ORIENTED_EDGE ( 'NONE', *, *, #5814, .T. ) ;
#18335 = ORIENTED_EDGE ( 'NONE', *, *, #6336, .F. ) ;
#18334 = ORIENTED_EDGE ( 'NONE', *, *, #18170, .F. ) ;
#18336 = CARTESIAN_POINT ( 'NONE',  ( -11.64274437364854187, -30.14459132904234195, 32.70117750791695244 ) ) ;
#18337 = VERTEX_POINT ( 'NONE', #13812 ) ;
#18338 = ORIENTED_EDGE ( 'NONE', *, *, #19370, .F. ) ;
#18339 = VECTOR ( 'NONE', #6001, 1000.000000000000000 ) ;
#18340 = VERTEX_POINT ( 'NONE', #16641 ) ;
#18341 = CARTESIAN_POINT ( 'NONE',  ( -14.83517299489736985, -26.99999999999998579, 19.36132249208304046 ) ) ;
#18342 = CARTESIAN_POINT ( 'NONE',  ( -11.35725562635144925, -18.02023567606020293, 15.20117750791695599 ) ) ;
#18343 = CARTESIAN_POINT ( 'NONE',  ( -2.066987300000000971, 63.14382582708704916, 47.20000000109248361 ) ) ;
#18344 = CARTESIAN_POINT ( 'NONE',  ( 2.500000000000001776, 64.00000000000000000, 49.60000000000000142 ) ) ;
#18345 = VERTEX_POINT ( 'NONE', #17196 ) ;
#18346 = CARTESIAN_POINT ( 'NONE',  ( -17.51566270880201159, -22.35725562635141728, 13.88867750791695954 ) ) ;
#18347 = CARTESIAN_POINT ( 'NONE',  ( -40.00000000000000711, 113.0000000000000000, 21.00000000000000000 ) ) ;
#18348 = ORIENTED_EDGE ( 'NONE', *, *, #4240, .T. ) ;
#18349 = CARTESIAN_POINT ( 'NONE',  ( -17.70357423236093553, -43.78611686177728046, 1.500000000000000000 ) ) ;
#18350 = ORIENTED_EDGE ( 'NONE', *, *, #9639, .T. ) ;
#18351 = LINE ( 'NONE', #10881, #5043 ) ;
#18352 = CARTESIAN_POINT ( 'NONE',  ( -0.1250000000000104083, 29.74264068711926257, 56.74264068711929809 ) ) ;
#18353 = DIRECTION ( 'NONE',  ( 0.000000000000000000, 0.7071067811865456854, 0.7071067811865494601 ) ) ;
#18354 = CYLINDRICAL_SURFACE ( 'NONE', #5800, 1.500000000000001332 ) ;
#18355 = VECTOR ( 'NONE', #10890, 1000.000000000000000 ) ;
#18356 = CARTESIAN_POINT ( 'NONE',  ( -0.8561741729129461742, 66.06698729999999387, 47.80000000109247082 ) ) ;
#18357 = ITEM_DEFINED_TRANSFORMATION ( 'NONE', 'NONE', #13932,  #1791 ) ;
#18358 = VECTOR ( 'NONE', #13880, 1000.000000000000000 ) ;
#18359 = FACE_OUTER_BOUND ( 'NONE', #3042, .T. ) ;
#18360 = CARTESIAN_POINT ( 'NONE',  ( -7.499999999999994671, -26.00000000000000355, 1.500000000000000000 ) ) ;
#18361 = EDGE_CURVE ( 'NONE', #291, #6660, #13489, .T. ) ;
#18362 = EDGE_CURVE ( 'NONE', #1647, #793, #11446, .T. ) ;
#18363 = CARTESIAN_POINT ( 'NONE',  ( 0.000000000000000000, 0.7390083445627224634, 1.279999999999999138 ) ) ;
#18364 = FACE_OUTER_BOUND ( 'NONE', #15192, .T. ) ;
#18365 = ORIENTED_EDGE ( 'NONE', *, *, #15060, .T. ) ;
#18367 = ADVANCED_FACE ( 'NONE', ( #6517 ), #15166, .F. ) ;
#18366 = CARTESIAN_POINT ( 'NONE',  ( -11.46040770435012668, -27.78091578003887463, 32.48242750791695954 ) ) ;
#18368 = LINE ( 'NONE', #18272, #18988 ) ;
#18369 = ORIENTED_EDGE ( 'NONE', *, *, #545, .T. ) ;
#18370 = CARTESIAN_POINT ( 'NONE',  ( -13.49542703274174116, -28.95583473709188738, 13.89257249208303691 ) ) ;
#18371 = ADVANCED_FACE ( 'NONE', ( #9539 ), #1443, .F. ) ;
#18372 = VECTOR ( 'NONE', #17011, 1000.000000000000114 ) ;
#18373 = VECTOR ( 'NONE', #15239, 1000.000000000000114 ) ;
#18374 = CARTESIAN_POINT ( 'NONE',  ( -17.51566270880199738, -25.64274437364856496, 20.23632249208304401 ) ) ;
#18375 = DIRECTION ( 'NONE',  ( -1.000000000000000000, -0.000000000000000000, -0.000000000000000000 ) ) ;
#18376 = ORIENTED_EDGE ( 'NONE', *, *, #14932, .F. ) ;
#18377 = LINE ( 'NONE', #332, #7175 ) ;
#18378 = ORIENTED_EDGE ( 'NONE', *, *, #7466, .F. ) ;
#18379 = CARTESIAN_POINT ( 'NONE',  ( -10.00000000000000000, -37.50000000000000000, 7.499999999999995559 ) ) ;
#18380 = CARTESIAN_POINT ( 'NONE',  ( 2.500000000000001776, 64.00000000000000000, 46.39999999999999858 ) ) ;
#18381 = CARTESIAN_POINT ( 'NONE',  ( -41.00000000000000711, 110.0000000000000000, 13.50000000000000000 ) ) ;
#18382 = CARTESIAN_POINT ( 'NONE',  ( -0.8561741729129466183, 61.93301270000000613, 45.10000000109246798 ) ) ;
#18383 = EDGE_CURVE ( 'NONE', #1809, #5878, #1539, .T. ) ;
#18384 = AXIS2_PLACEMENT_3D ( 'NONE', #11574, #14626, #16096 ) ;
#18385 = CIRCLE ( 'NONE', #5840, 0.1000000000000000472 ) ;
#18386 = PLANE ( 'NONE',  #14148 ) ;
#18387 = FACE_OUTER_BOUND ( 'NONE', #5243, .T. ) ;
#18388 = ORIENTED_EDGE ( 'NONE', *, *, #5288, .F. ) ;
#18389 = CARTESIAN_POINT ( 'NONE',  ( -19.95583473709191580, -22.49542703274176603, 13.66992750791695599 ) ) ;
#18390 = CARTESIAN_POINT ( 'NONE',  ( -2.500000000000001776, 65.03553390593273775, 46.85000000218494165 ) ) ;
#18391 = CARTESIAN_POINT ( 'NONE',  ( -19.24771351637086880, -26.64274437364857206, 14.98632249208304046 ) ) ;
#18392 =( BOUNDED_CURVE ( )  B_SPLINE_CURVE ( 2, ( #9922, #17587, #14346, #17208, #15634, #6809, #3774, #2482, #2300 ),
 .UNSPECIFIED., .F., .F. ) 
 B_SPLINE_CURVE_WITH_KNOTS ( ( 3, 2, 2, 2, 3 ),
 ( 0.4285714285714284366, 0.4464285714285713413, 0.4642857142857141906, 0.4821428571428570953, 0.4999999999999999445 ),
 .UNSPECIFIED. ) 
 CURVE ( )  GEOMETRIC_REPRESENTATION_ITEM ( )  RATIONAL_B_SPLINE_CURVE ( ( 1.000000000000000444, 0.9238795325112862944, 1.000000000000000000, 0.9238795325112867385, 1.000000000000000000, 0.9238795325112867385, 1.000000000000000000, 0.9238795325112869605, 0.9999999999999997780 ) ) 
 REPRESENTATION_ITEM ( '' )  );
#18393 = EDGE_CURVE ( 'NONE', #1736, #3722, #11104, .T. ) ;
#18394 = EDGE_CURVE ( 'NONE', #13522, #10477, #9636, .T. ) ;
#18395 = PLANE ( 'NONE',  #13849 ) ;
#18396 = CARTESIAN_POINT ( 'NONE',  ( -10.04416526290807710, -25.50457296725819489, 16.29492750791695954 ) ) ;
#18397 = EDGE_CURVE ( 'NONE', #12335, #12613, #3667, .T. ) ;
#18398 = CARTESIAN_POINT ( 'NONE',  ( 7.500000000000005329, -26.00000000000000000, 4.500000000000000888 ) ) ;
#18399 = CARTESIAN_POINT ( 'NONE',  ( -16.50457296725820555, -28.95583473709189803, 12.35742750791695777 ) ) ;
#18400 = DIRECTION ( 'NONE',  ( 2.312964634635742957E-16, -1.000000000000000000, 0.000000000000000000 ) ) ;
#18401 = CARTESIAN_POINT ( 'NONE',  ( -11.21908421996106142, -27.53959229564982181, 18.70507249208304401 ) ) ;
#18402 = CARTESIAN_POINT ( 'NONE',  ( 0.8561741729129460632, 66.06698729999999387, 48.70000000109247651 ) ) ;
#18403 = CARTESIAN_POINT ( 'NONE',  ( 2.500000000000011102, 62.96446609406727646, 49.54999999999999716 ) ) ;
#18404 = LINE ( 'NONE', #7807, #16013 ) ;
#18405 = DIRECTION ( 'NONE',  ( -0.000000000000000000, -1.000000000000000000, -0.000000000000000000 ) ) ;
#18406 = CARTESIAN_POINT ( 'NONE',  ( -0.8561741729129465073, 61.93301270000000613, 47.50000000109246656 ) ) ;
#18407 = CARTESIAN_POINT ( 'NONE',  ( 0.000000000000000000, 0.000000000000000000, 4.000000000000000000 ) ) ;
#18408 = VERTEX_POINT ( 'NONE', #6051 ) ;
#18409 = VERTEX_POINT ( 'NONE', #17101 ) ;
#18410 = CARTESIAN_POINT ( 'NONE',  ( -7.955834737091903364, -25.71081734191518464, 34.01757249208303335 ) ) ;
#18411 = SURFACE_STYLE_USAGE ( .BOTH. , #10547 ) ;
#18412 = CARTESIAN_POINT ( 'NONE',  ( -17.35725562635140307, -28.41254052147349185, 14.54882249208304046 ) ) ;
#18413 = ORIENTED_EDGE ( 'NONE', *, *, #12935, .F. ) ;
#18414 = ADVANCED_FACE ( 'NONE', ( #9082 ), #18010, .T. ) ;
#18415 = CARTESIAN_POINT ( 'NONE',  ( -17.99999999999999645, -23.83517299489736985, 34.45117750791695954 ) ) ;
#18416 = EDGE_CURVE ( 'NONE', #12636, #8015, #14153, .T. ) ;
#18417 = PLANE ( 'NONE',  #3316 ) ;
#18418 = CARTESIAN_POINT ( 'NONE',  ( -21.99999999999999289, -24.16482700510262305, 25.92382249208304046 ) ) ;
#18419 = CARTESIAN_POINT ( 'NONE',  ( -0.8561741729129465073, 61.93301270000000613, 45.70000000109248361 ) ) ;
#18420 = CARTESIAN_POINT ( 'NONE',  ( -0.8561741729129465073, 61.93301270000000613, 45.70000000109248361 ) ) ;
#18421 = ORIENTED_EDGE ( 'NONE', *, *, #1921, .T. ) ;
#18422 = VERTEX_POINT ( 'NONE', #814 ) ;
#18423 = CARTESIAN_POINT ( 'NONE',  ( -1.767766952966370209, 65.76776695296638309, 46.00000000218494733 ) ) ;
#18424 = CARTESIAN_POINT ( 'NONE',  ( -50.00000000000001421, 3.000000000000000000, 59.99999999999997868 ) ) ;
#18425 = CARTESIAN_POINT ( 'NONE',  ( -40.00000000000000000, 53.00000000000000711, 30.00000000000000000 ) ) ;
#18426 = CARTESIAN_POINT ( 'NONE',  ( -4.012830983233701687, 26.60336399182265055, 59.52836399182262994 ) ) ;
#18427 = FACE_OUTER_BOUND ( 'NONE', #13584, .T. ) ;
#18428 = DIRECTION ( 'NONE',  ( -7.709882115452476934E-17, 0.000000000000000000, -1.000000000000000000 ) ) ;
#18429 = CARTESIAN_POINT ( 'NONE',  ( -2.499999999999992450, 65.03553390593275196, 47.65000000218494591 ) ) ;
#18430 = VERTEX_POINT ( 'NONE', #11477 ) ;
#18432 = ORIENTED_EDGE ( 'NONE', *, *, #18890, .T. ) ;
#18431 = ORIENTED_EDGE ( 'NONE', *, *, #11049, .T. ) ;
#18433 = CARTESIAN_POINT ( 'NONE',  ( -14.83517299489740715, -16.99999999999997868, 35.76367750791694533 ) ) ;
#18434 = ORIENTED_EDGE ( 'NONE', *, *, #16636, .F. ) ;
#18435 = EDGE_LOOP ( 'NONE', ( #13396, #7635, #5996, #4701 ) ) ;
#18436 = EDGE_CURVE ( 'NONE', #10380, #2146, #17373, .T. ) ;
#18437 = CARTESIAN_POINT ( 'NONE',  ( -12.68318583509882380, -26.07549068051207541, 29.20507249208304756 ) ) ;
#18438 = CARTESIAN_POINT ( 'NONE',  ( -8.855408670957631401, -20.64274437364852943, 20.88867750791695954 ) ) ;
#18439 = AXIS2_PLACEMENT_3D ( 'NONE', #12687, #13975, #15548 ) ;
#18440 = PLANE ( 'NONE',  #17831 ) ;
#18441 = LINE ( 'NONE', #2153, #11881 ) ;
#18442 = ORIENTED_EDGE ( 'NONE', *, *, #18042, .F. ) ;
#18443 = CARTESIAN_POINT ( 'NONE',  ( -11.95583473709191047, -23.36097942780921954, 36.85742750791697375 ) ) ;
#18444 = ORIENTED_EDGE ( 'NONE', *, *, #12621, .T. ) ;
#18445 = DIRECTION ( 'NONE',  ( -0.000000000000000000, -0.000000000000000000, -1.000000000000000000 ) ) ;
#18446 = ORIENTED_EDGE ( 'NONE', *, *, #16711, .F. ) ;
#18447 = CARTESIAN_POINT ( 'NONE',  ( -37.50000000000002132, 0.000000000000000000, -25.00000000000002132 ) ) ;
#18448 = DIRECTION ( 'NONE',  ( 0.000000000000000000, -1.000000000000000000, 0.000000000000000000 ) ) ;
#18449 = DIRECTION ( 'NONE',  ( 1.734723475976807094E-15, -1.000000000000000000, 0.000000000000000000 ) ) ;
#18450 = CARTESIAN_POINT ( 'NONE',  ( 2.492551403682577771, 31.38014068711926541, 55.10514068711930236 ) ) ;
#18451 = FACE_OUTER_BOUND ( 'NONE', #9341, .T. ) ;
#18452 = ITEM_DEFINED_TRANSFORMATION ( 'NONE', 'NONE', #1088,  #1791 ) ;
#18453 = CARTESIAN_POINT ( 'NONE',  ( 13.49999999999992362, 39.11180553784094371, 47.01992244580438296 ) ) ;
#18454 = CARTESIAN_POINT ( 'NONE',  ( -32.50000000000000000, 53.00000000000000711, 12.35000000000000675 ) ) ;
#18455 = VECTOR ( 'NONE', #5845, 1000.000000000000000 ) ;
#18456 = CARTESIAN_POINT ( 'NONE',  ( -9.120482147295685276E-15, 33.84386001800124433, 52.64142135623733054 ) ) ;
#18457 = CARTESIAN_POINT ( 'NONE',  ( 2.500000000000000000, 0.000000000000000000, 2.041999999999999815 ) ) ;
#18458 = ORIENTED_EDGE ( 'NONE', *, *, #654, .T. ) ;
#18459 = CARTESIAN_POINT ( 'NONE',  ( -9.955834737091912245, -22.82508104294696594, 31.60742750791695954 ) ) ;
#18460 = DIRECTION ( 'NONE',  ( 0.000000000000000000, -1.000000000000000000, 0.000000000000000000 ) ) ;
#18461 = ADVANCED_FACE ( 'NONE', ( #5612 ), #2379, .T. ) ;
#18462 = VERTEX_POINT ( 'NONE', #17288 ) ;
#18463 = EDGE_CURVE ( 'NONE', #4643, #5010, #17464, .T. ) ;
#18464 = CARTESIAN_POINT ( 'NONE',  ( -20.04416526290809131, -22.82508104294699791, 36.64257249208304046 ) ) ;
#18465 = CIRCLE ( 'NONE', #7800, 7.000000000000004441 ) ;
#18466 = CARTESIAN_POINT ( 'NONE',  ( -12.48433729119799196, -22.35725562635139596, 12.36132249208304401 ) ) ;
#18467 = LINE ( 'NONE', #5229, #16929 ) ;
#18468 = ORIENTED_EDGE ( 'NONE', *, *, #4980, .F. ) ;
#18469 = VECTOR ( 'NONE', #9385, 1000.000000000000000 ) ;
#18470 = CARTESIAN_POINT ( 'NONE',  ( 0.000000000000000000, 47.00000000000000711, 30.00000000000000000 ) ) ;
#18471 = VERTEX_POINT ( 'NONE', #5513 ) ;
#18472 = CARTESIAN_POINT ( 'NONE',  ( 1.300000000000000044, -1.478016689125442706, 1.843143693225357538E-15 ) ) ;
#18473 = LINE ( 'NONE', #6318, #12048 ) ;
#18474 = LINE ( 'NONE', #9337, #6619 ) ;
#18475 = CARTESIAN_POINT ( 'NONE',  ( -2.500000000000001776, 64.00000000000000000, 49.65000000109247225 ) ) ;
#18476 = VECTOR ( 'NONE', #13320, 1000.000000000000000 ) ;
#18477 = CARTESIAN_POINT ( 'NONE',  ( 2.500000000000001776, 64.00000000000000000, 46.39999999999999858 ) ) ;
#18478 = CARTESIAN_POINT ( 'NONE',  ( 2.500000000000000000, 2.357898499370431722, -2.818925648462311528E-15 ) ) ;
#18479 = ADVANCED_FACE ( 'NONE', ( #18758 ), #11292, .T. ) ;
#18480 = CARTESIAN_POINT ( 'NONE',  ( -44.99999999999998579, 3.000000000000000000, -55.00000000000000000 ) ) ;
#18481 = VECTOR ( 'NONE', #4844, 1000.000000000000000 ) ;
#18482 = DIRECTION ( 'NONE',  ( 0.000000000000000000, 0.000000000000000000, -1.000000000000000000 ) ) ;
#18483 = VECTOR ( 'NONE', #7507, 1000.000000000000000 ) ;
#18484 = ORIENTED_EDGE ( 'NONE', *, *, #10674, .F. ) ;
#18485 = CARTESIAN_POINT ( 'NONE',  ( -12.64274437364855252, -28.41254052147347053, 22.20117750791695599 ) ) ;
#18486 = VECTOR ( 'NONE', #14584, 1000.000000000000000 ) ;
#18487 = CARTESIAN_POINT ( 'NONE',  ( 2.500000000000002220, 62.96446609406726935, 44.85000000218494165 ) ) ;
#18488 = ADVANCED_FACE ( 'NONE', ( #10005 ), #12949, .T. ) ;
#18489 = CARTESIAN_POINT ( 'NONE',  ( -14.83517299489735741, -28.99999999999998224, 14.11132249208304046 ) ) ;
#18490 = VECTOR ( 'NONE', #14365, 1000.000000000000000 ) ;
#18491 = DIRECTION ( 'NONE',  ( -0.000000000000000000, -1.000000000000000000, -0.000000000000000000 ) ) ;
#18492 = CARTESIAN_POINT ( 'NONE',  ( -12.35725562635143682, -19.75228648362908501, 20.45117750791695954 ) ) ;
#18493 = CARTESIAN_POINT ( 'NONE',  ( 32.50000000000000000, 47.00000000000000711, 17.49999999999999645 ) ) ;
#18494 = CARTESIAN_POINT ( 'NONE',  ( -13.49542703274178201, -19.04416526290806289, 30.73242750791695954 ) ) ;
#18495 = VECTOR ( 'NONE', #1779, 1000.000000000000000 ) ;
#18496 = CARTESIAN_POINT ( 'NONE',  ( 1.300000000000000044, -1.314525273895014473E-15, -1.280000000000000027 ) ) ;
#18497 = CARTESIAN_POINT ( 'NONE',  ( -14.83517299489735741, -28.99999999999998224, 29.86132249208304401 ) ) ;
#18498 = CARTESIAN_POINT ( 'NONE',  ( 2.066987300000002303, 63.14382582708705627, 49.30000000109246372 ) ) ;
#18499 = CARTESIAN_POINT ( 'NONE',  ( -2.750000000000020872, 118.0000000000000142, 37.49999999999997158 ) ) ;
#18500 = FACE_OUTER_BOUND ( 'NONE', #15777, .T. ) ;
#18501 = VECTOR ( 'NONE', #7678, 1000.000000000000000 ) ;
#18502 = CARTESIAN_POINT ( 'NONE',  ( 0.8561741729129460632, 66.06698729999999387, 48.70000000109247651 ) ) ;
#18503 = DIRECTION ( 'NONE',  ( 1.000000000000000000, -0.000000000000000000, -0.000000000000000000 ) ) ;
#18504 = AXIS2_PLACEMENT_3D ( 'NONE', #10548, #11818, #13587 ) ;
#18505 = ADVANCED_FACE ( 'NONE', ( #8273 ), #9730, .T. ) ;
#18506 = ORIENTED_EDGE ( 'NONE', *, *, #9790, .F. ) ;
#18507 = ORIENTED_EDGE ( 'NONE', *, *, #17753, .F. ) ;
#18508 = ADVANCED_FACE ( 'NONE', ( #14525 ), #1096, .T. ) ;
#18509 = CARTESIAN_POINT ( 'NONE',  ( -11.35725562635139418, -29.97976432393972601, 34.67382249208304046 ) ) ;
#18510 = CONICAL_SURFACE ( 'NONE', #2206, 2.041999999999999815, 1.047197551196591858 ) ;
#18511 = CARTESIAN_POINT ( 'NONE',  ( -11.21908421996106142, -27.53959229564982181, 13.45507249208304223 ) ) ;
#18512 = EDGE_LOOP ( 'NONE', ( #12410, #14888, #11466 ) ) ;
#18513 = CARTESIAN_POINT ( 'NONE',  ( -12.31951028609537602, -22.64274437364854364, 31.38867750791696309 ) ) ;
#18514 = DIRECTION ( 'NONE',  ( 0.000000000000000000, -1.000000000000000000, 0.000000000000000000 ) ) ;
#18515 = CARTESIAN_POINT ( 'NONE',  ( -9.754982604823302594, -29.00369391078756465, 18.70507249208304046 ) ) ;
#18516 = STYLED_ITEM ( 'NONE', ( #2156 ), #3958 ) ;
#18517 = CARTESIAN_POINT ( 'NONE',  ( 1.461580736456473684, 65.46158073645646880, 46.85000000109246798 ) ) ;
#18518 = FACE_OUTER_BOUND ( 'NONE', #14434, .T. ) ;
#18519 = EDGE_LOOP ( 'NONE', ( #13263, #13648, #18421, #9678 ) ) ;
#18520 = ORIENTED_EDGE ( 'NONE', *, *, #15915, .F. ) ;
#18521 = CARTESIAN_POINT ( 'NONE',  ( -50.00000000000002132, 118.0000000000000142, 37.49999999999997868 ) ) ;
#18522 = DIRECTION ( 'NONE',  ( -1.000000000000000000, 0.000000000000000000, 0.000000000000000000 ) ) ;
#18523 = AXIS2_PLACEMENT_3D ( 'NONE', #14821, #2074, #15305 ) ;
#18524 = CARTESIAN_POINT ( 'NONE',  ( -1.461580736456473462, 62.53841926354353120, 48.05000000109247082 ) ) ;
#18525 = CARTESIAN_POINT ( 'NONE',  ( -24.00000000000000000, 52.00000000000000711, -50.00000000000000000 ) ) ;
#18526 = AXIS2_PLACEMENT_3D ( 'NONE', #4657, #18187, #3180 ) ;
#18527 = CARTESIAN_POINT ( 'NONE',  ( 13.49999999999981348, 20.01992244580421598, 66.11180553784100766 ) ) ;
#18528 = DIRECTION ( 'NONE',  ( 5.782411586589357392E-17, -0.000000000000000000, 1.000000000000000000 ) ) ;
#18529 = VECTOR ( 'NONE', #11940, 1000.000000000000000 ) ;
#18530 = ADVANCED_FACE ( 'NONE', ( #15812 ), #8365, .F. ) ;
#18531 = DIRECTION ( 'NONE',  ( 0.000000000000000000, -1.000000000000000000, -0.000000000000000000 ) ) ;
#18532 = ORIENTED_EDGE ( 'NONE', *, *, #11425, .F. ) ;
#18533 = ORIENTED_EDGE ( 'NONE', *, *, #9649, .F. ) ;
#18534 = CARTESIAN_POINT ( 'NONE',  ( -21.95583473709191580, -21.95952864787954084, 29.41992750791695954 ) ) ;
#18535 = ORIENTED_EDGE ( 'NONE', *, *, #9857, .F. ) ;
#18537 = ORIENTED_EDGE ( 'NONE', *, *, #14625, .F. ) ;
#18536 = ORIENTED_EDGE ( 'NONE', *, *, #3289, .T. ) ;
#18538 = CARTESIAN_POINT ( 'NONE',  ( -17.31681416490117087, -21.92450931948788551, 31.83007249208304046 ) ) ;
#18539 = EDGE_CURVE ( 'NONE', #793, #1647, #10526, .T. ) ;
#18540 = CARTESIAN_POINT ( 'NONE',  ( -21.99999999999999289, -23.83517299489739116, 23.95117750791696309 ) ) ;
#18541 = COLOUR_RGB ( '', 0.08235294, 0.09019608, 0.10196078) ;
#18542 = CARTESIAN_POINT ( 'NONE',  ( -41.00000000000000000, 52.00000000000000711, 30.00000000000000000 ) ) ;
#18543 = DIRECTION ( 'NONE',  ( 1.000000000000000000, 0.000000000000000000, 0.000000000000000000 ) ) ;
#18544 = CARTESIAN_POINT ( 'NONE',  ( 0.1249999999999895917, 31.97002704785689531, 54.16170093578840294 ) ) ;
#18545 = ORIENTED_EDGE ( 'NONE', *, *, #8362, .F. ) ;
#18546 = CARTESIAN_POINT ( 'NONE',  ( -17.07549068051210739, -21.68318583509881847, 24.60742750791696309 ) ) ;
#18547 = LINE ( 'NONE', #5114, #17556 ) ;
#18548 = EDGE_LOOP ( 'NONE', ( #13762, #5088, #10076, #19325 ) ) ;
#18549 = DIRECTION ( 'NONE',  ( -1.000000000000000000, 0.000000000000000000, 0.000000000000000000 ) ) ;
#18550 = VERTEX_POINT ( 'NONE', #8643 ) ;
#18551 = LINE ( 'NONE', #14019, #2546 ) ;
#18552 = LINE ( 'NONE', #9318, #13090 ) ;
#18553 = CARTESIAN_POINT ( 'NONE',  ( -50.00000000000002132, 118.0000000000000142, 37.49999999999997868 ) ) ;
#18554 = CARTESIAN_POINT ( 'NONE',  ( 2.315774708385922587, 27.98014068711924551, 58.50514068711930804 ) ) ;
#18555 = DIRECTION ( 'NONE',  ( 0.000000000000000000, 0.000000000000000000, -1.000000000000000000 ) ) ;
#18556 = CONTEXT_DEPENDENT_SHAPE_REPRESENTATION ( #9068, #9868 ) ;
#18557 = EDGE_CURVE ( 'NONE', #6502, #10761, #19040, .T. ) ;
#18558 = CARTESIAN_POINT ( 'NONE',  ( 1.461580736456473906, 62.53841926354353120, 47.65000000109247225 ) ) ;
#18559 = CARTESIAN_POINT ( 'NONE',  ( -44.99999999999998579, 3.000000000000000000, -56.59999999999999432 ) ) ;
#18560 = PLANE ( 'NONE',  #3964 ) ;
#18561 = LINE ( 'NONE', #13736, #12389 ) ;
#18562 = ORIENTED_EDGE ( 'NONE', *, *, #5773, .F. ) ;
#18563 = CARTESIAN_POINT ( 'NONE',  ( -19.24771351637089367, -21.35725562635142438, 34.88867750791696665 ) ) ;
#18564 = CARTESIAN_POINT ( 'NONE',  ( 2.500000000000000000, -1.178949249685214307, 2.042000000000002036 ) ) ;
#18565 = ORIENTED_EDGE ( 'NONE', *, *, #3664, .F. ) ;
#18566 = CARTESIAN_POINT ( 'NONE',  ( -17.35725562635140307, -28.41254052147349185, 25.04882249208304401 ) ) ;
#18567 = EDGE_CURVE ( 'NONE', #18051, #1372, #19304, .T. ) ;
#18568 = CARTESIAN_POINT ( 'NONE',  ( -13.64274437364857739, -21.31951028609534760, 32.92382249208304046 ) ) ;
#18569 = CARTESIAN_POINT ( 'NONE',  ( -41.00000000000000711, 110.0000000000000000, 26.50000000000000000 ) ) ;
#18570 = VERTEX_POINT ( 'NONE', #12763 ) ;
#18571 = LINE ( 'NONE', #11094, #2178 ) ;
#18572 = ORIENTED_EDGE ( 'NONE', *, *, #15426, .F. ) ;
#18573 = DIRECTION ( 'NONE',  ( 0.000000000000000000, 0.4999999999999991673, -0.8660254037844391517 ) ) ;
#18574 = DIRECTION ( 'NONE',  ( 1.000000000000000000, -0.000000000000000000, -0.000000000000000000 ) ) ;
#18575 = AXIS2_PLACEMENT_3D ( 'NONE', #18611, #17043, #5176 ) ;
#18576 = DIRECTION ( 'NONE',  ( 0.000000000000000000, -0.7071067811865493491, 0.7071067811865456854 ) ) ;
#18577 = CYLINDRICAL_SURFACE ( 'NONE', #362, 2.500000000000002220 ) ;
#18578 = DIRECTION ( 'NONE',  ( 0.000000000000000000, 0.000000000000000000, -1.000000000000000000 ) ) ;
#18579 = DIRECTION ( 'NONE',  ( 0.000000000000000000, 0.000000000000000000, -1.000000000000000000 ) ) ;
#18580 = VERTEX_POINT ( 'NONE', #905 ) ;
#18581 = CARTESIAN_POINT ( 'NONE',  ( -17.35725562635144215, -19.58745947852648683, 24.82617750791695954 ) ) ;
#18582 = CARTESIAN_POINT ( 'NONE',  ( -1.035533905932738641, 66.50000000000000000, 45.95000000218494307 ) ) ;
#18583 = CARTESIAN_POINT ( 'NONE',  ( -10.75228648362912232, -21.35725562635138530, 28.11132249208304046 ) ) ;
#18584 = LINE ( 'NONE', #14162, #8441 ) ;
#18585 = CARTESIAN_POINT ( 'NONE',  ( -17.64274437364855430, -28.24771351637087236, 17.82617750791695599 ) ) ;
#18586 = CARTESIAN_POINT ( 'NONE',  ( -32.50000000000000000, 47.00000000000000711, 17.49999999999999645 ) ) ;
#18587 = CARTESIAN_POINT ( 'NONE',  ( -13.82508104294698015, -29.04416526290806289, 32.91992750791695954 ) ) ;
#18588 = CARTESIAN_POINT ( 'NONE',  ( 9.339266095310328808, -43.78611686177728046, 1.500000000000000000 ) ) ;
#18589 = CARTESIAN_POINT ( 'NONE',  ( -19.24771351637086880, -26.64274437364857206, 25.48632249208304401 ) ) ;
#18590 = CARTESIAN_POINT ( 'NONE',  ( -2.066987300000001415, 63.14382582708705627, 45.80000000109246372 ) ) ;
#18591 = LINE ( 'NONE', #9269, #6538 ) ;
#18592 = CARTESIAN_POINT ( 'NONE',  ( -32.50000000000000000, 52.00000000000000711, -35.00000000000000000 ) ) ;
#18593 = CARTESIAN_POINT ( 'NONE',  ( -41.00000000000000711, 53.00000000000000711, -37.50000000000000711 ) ) ;
#18594 = CARTESIAN_POINT ( 'NONE',  ( 2.066987300000001859, 64.85617417291294373, 47.00000000109246656 ) ) ;
#18595 = EDGE_CURVE ( 'NONE', #4896, #17611, #19143, .T. ) ;
#18596 = EDGE_CURVE ( 'NONE', #17276, #14706, #12859, .T. ) ;
#18597 = DIRECTION ( 'NONE',  ( 0.000000000000000000, 0.000000000000000000, -1.000000000000000000 ) ) ;
#18598 = VERTEX_POINT ( 'NONE', #18947 ) ;
#18599 = CARTESIAN_POINT ( 'NONE',  ( -22.04416526290809486, -22.28918265808477628, 31.39257249208304401 ) ) ;
#18600 = EDGE_CURVE ( 'NONE', #11781, #11383, #5425, .T. ) ;
#18601 = FILL_AREA_STYLE ('',( #17034 ) ) ;
#18602 = CARTESIAN_POINT ( 'NONE',  ( 2.066987300000001415, 64.85617417291294373, 46.00000000109247367 ) ) ;
#18603 = CARTESIAN_POINT ( 'NONE',  ( -13.35725562635142794, -21.48433729119796709, 25.70117750791695954 ) ) ;
#18604 = CARTESIAN_POINT ( 'NONE',  ( -25.00000000000000000, 110.0000000000000000, 1.500000000000001332 ) ) ;
#18605 = EDGE_CURVE ( 'NONE', #7333, #13130, #8457, .T. ) ;
#18606 = CARTESIAN_POINT ( 'NONE',  ( -21.95583473709189803, -26.04047135212049469, 20.45507249208304046 ) ) ;
#18607 = CARTESIAN_POINT ( 'NONE',  ( -0.8561741729129461742, 66.06698729999999387, 46.20000000109247651 ) ) ;
#18608 = EDGE_LOOP ( 'NONE', ( #16617, #1105, #12765, #10543, #7679 ) ) ;
#18609 = ORIENTED_EDGE ( 'NONE', *, *, #9935, .F. ) ;
#18610 = DIRECTION ( 'NONE',  ( 1.000000000000000000, 0.000000000000000000, 0.000000000000000000 ) ) ;
#18611 = CARTESIAN_POINT ( 'NONE',  ( -32.50000000000000000, 52.00000000000000711, 15.00000000000000000 ) ) ;
#18612 = CARTESIAN_POINT ( 'NONE',  ( -2.066987300000001415, 64.85617417291294373, 46.30000000109247082 ) ) ;
#18613 = DIRECTION ( 'NONE',  ( -0.000000000000000000, 1.000000000000000000, -0.000000000000000000 ) ) ;
#18614 = EDGE_CURVE ( 'NONE', #9379, #18899, #4273, .T. ) ;
#18615 = CARTESIAN_POINT ( 'NONE',  ( -7.499999999999994671, -38.00000000000000000, 1.500000000000000000 ) ) ;
#18616 = VECTOR ( 'NONE', #10908, 1000.000000000000000 ) ;
#18617 = CARTESIAN_POINT ( 'NONE',  ( -41.00000000000000711, 53.00000000000000711, 0.5000000000000004441 ) ) ;
#18618 = CARTESIAN_POINT ( 'NONE',  ( -24.00000000000000000, 110.0000000000000000, 0.5000000000000004441 ) ) ;
#18619 = ORIENTED_EDGE ( 'NONE', *, *, #12623, .T. ) ;
#18620 = EDGE_CURVE ( 'NONE', #16642, #14902, #15024, .T. ) ;
#18621 = ORIENTED_EDGE ( 'NONE', *, *, #8922, .T. ) ;
#18622 = CARTESIAN_POINT ( 'NONE',  ( -20.97976432393977575, -20.35725562635143504, 34.88867750791695954 ) ) ;
#18623 =( NAMED_UNIT ( * ) SI_UNIT ( $, .STERADIAN. ) SOLID_ANGLE_UNIT ( ) );
#18624 = ORIENTED_EDGE ( 'NONE', *, *, #4091, .T. ) ;
#18626 = ORIENTED_EDGE ( 'NONE', *, *, #3003, .T. ) ;
#18625 = EDGE_LOOP ( 'NONE', ( #4500, #8413, #8480, #611 ) ) ;
#18627 = CARTESIAN_POINT ( 'NONE',  ( -17.51566270880199738, -25.64274437364856496, 30.73632249208304401 ) ) ;
#18628 = CARTESIAN_POINT ( 'NONE',  ( -21.14459132904236327, -27.35725562635143149, 13.01367750791695777 ) ) ;
#18629 = CIRCLE ( 'NONE', #10137, 1.219500000000000028 ) ;
#18630 = FACE_OUTER_BOUND ( 'NONE', #5884, .T. ) ;
#18631 = CARTESIAN_POINT ( 'NONE',  ( -1.767766952966369765, 62.23223304703363112, 47.80000000218494449 ) ) ;
#18632 = DIRECTION ( 'NONE',  ( -0.000000000000000000, -1.000000000000000000, -0.000000000000000000 ) ) ;
#18633 = ORIENTED_EDGE ( 'NONE', *, *, #4704, .T. ) ;
#18634 = CARTESIAN_POINT ( 'NONE',  ( -11.95583473709191047, -23.36097942780921954, 26.35742750791696309 ) ) ;
#18635 = CARTESIAN_POINT ( 'NONE',  ( -50.00000000000002132, 33.00000000000000000, 59.99999999999997868 ) ) ;
#18636 = ORIENTED_EDGE ( 'NONE', *, *, #5881, .T. ) ;
#18637 = EDGE_CURVE ( 'NONE', #5590, #12626, #6105, .T. ) ;
#18638 = EDGE_CURVE ( 'NONE', #15185, #5969, #223, .T. ) ;
#18639 = DIRECTION ( 'NONE',  ( -4.088782444488986608E-17, 0.7071067811865495711, -0.7071067811865455743 ) ) ;
#18640 = ORIENTED_EDGE ( 'NONE', *, *, #2101, .F. ) ;
#18641 = LINE ( 'NONE', #12262, #11938 ) ;
#18642 = DIRECTION ( 'NONE',  ( -1.000000000000000000, 0.000000000000000000, -0.000000000000000000 ) ) ;
#18643 = DIRECTION ( 'NONE',  ( 0.000000000000000000, 0.000000000000000000, -1.000000000000000000 ) ) ;
#18644 = ADVANCED_FACE ( 'NONE', ( #6208 ), #6010, .T. ) ;
#18645 = CARTESIAN_POINT ( 'NONE',  ( 0.8561741729129472844, 61.93301270000000613, 47.40000000109247225 ) ) ;
#18646 = EDGE_CURVE ( 'NONE', #8851, #11032, #207, .T. ) ;
#18647 = CARTESIAN_POINT ( 'NONE',  ( 1.461580736456473906, 62.53841926354353120, 46.85000000109246798 ) ) ;
#18648 = CYLINDRICAL_SURFACE ( 'NONE', #7205, 2.500000000000001776 ) ;
#18649 = CARTESIAN_POINT ( 'NONE',  ( -37.50000000000002842, -6.000000000000000000, -47.50000000000002132 ) ) ;
#18650 = CARTESIAN_POINT ( 'NONE',  ( -1.035533905932738641, 66.50000000000000000, 49.85000000000000853 ) ) ;
#18651 = AXIS2_PLACEMENT_3D ( 'NONE', #11857, #17958, #10392 ) ;
#18652 = CARTESIAN_POINT ( 'NONE',  ( 1.466517438298505116, 62.42153833278998576, 44.99999999999999289 ) ) ;
#18653 = EDGE_LOOP ( 'NONE', ( #9626, #12391 ) ) ;
#18654 = ORIENTED_EDGE ( 'NONE', *, *, #14543, .T. ) ;
#18655 = CARTESIAN_POINT ( 'NONE',  ( -19.95583473709191580, -22.49542703274176603, 24.16992750791694888 ) ) ;
#18656 = CARTESIAN_POINT ( 'NONE',  ( -45.00000000000000000, 3.000000000000000000, 54.99999999999998579 ) ) ;
#18657 = ORIENTED_EDGE ( 'NONE', *, *, #7350, .T. ) ;
#18658 = CARTESIAN_POINT ( 'NONE',  ( -13.82508104294702100, -18.95583473709188382, 27.45507249208304046 ) ) ;
#18659 = DIRECTION ( 'NONE',  ( -3.826732013112564095E-16, 1.000000000000000000, 1.632680918566406793E-16 ) ) ;
#18660 = ADVANCED_FACE ( 'NONE', ( #4339 ), #16193, .T. ) ;
#18661 = CARTESIAN_POINT ( 'NONE',  ( -12.92450931948790149, -21.68318583509881137, 27.89257249208304401 ) ) ;
#18662 = CIRCLE ( 'NONE', #8023, 2.500000000000002220 ) ;
#18663 = DIRECTION ( 'NONE',  ( -1.000000000000000000, -0.000000000000000000, -0.000000000000000000 ) ) ;
#18664 = VERTEX_POINT ( 'NONE', #9139 ) ;
#18665 = VECTOR ( 'NONE', #18503, 1000.000000000000000 ) ;
#18666 = CARTESIAN_POINT ( 'NONE',  ( -25.00000000000000000, 110.0000000000000000, -31.00000000000000000 ) ) ;
#18667 = VERTEX_POINT ( 'NONE', #10496 ) ;
#18668 = CARTESIAN_POINT ( 'NONE',  ( -3.065533689247737392, -45.28611686177728046, 3.000000000000000000 ) ) ;
#18669 = DIRECTION ( 'NONE',  ( 1.000000000000000000, 0.000000000000000000, -0.000000000000000000 ) ) ;
#18670 = CARTESIAN_POINT ( 'NONE',  ( 2.500000000000001776, 65.03553390593273775, 45.75000000218494733 ) ) ;
#18671 = FACE_OUTER_BOUND ( 'NONE', #7884, .T. ) ;
#18672 = CARTESIAN_POINT ( 'NONE',  ( -25.00000000000000711, 110.0000000000000000, -19.00000000000000000 ) ) ;
#18673 = CARTESIAN_POINT ( 'NONE',  ( 0.000000000000000000, 118.0000000000000142, 0.000000000000000000 ) ) ;
#18674 = CIRCLE ( 'NONE', #13324, 2.500000000000002220 ) ;
#18675 = CARTESIAN_POINT ( 'NONE',  ( -25.00000000000000711, 53.00000000000000711, -11.50000000000000000 ) ) ;
#18676 = VECTOR ( 'NONE', #5634, 1000.000000000000000 ) ;
#18677 = ORIENTED_EDGE ( 'NONE', *, *, #2549, .F. ) ;
#18678 = CARTESIAN_POINT ( 'NONE',  ( -20.04416526290808065, -25.17491895705300209, 34.23242750791695954 ) ) ;
#18679 = EDGE_CURVE ( 'NONE', #14101, #834, #13242, .T. ) ;
#18680 = CARTESIAN_POINT ( 'NONE',  ( -0.8561741729129461742, 66.06698729999999387, 49.40000000109247225 ) ) ;
#18681 = CARTESIAN_POINT ( 'NONE',  ( -17.35725562635140307, -28.41254052147349185, 30.29882249208304401 ) ) ;
#18682 = DIRECTION ( 'NONE',  ( 0.000000000000000000, -0.8660254037844390407, -0.4999999999999994449 ) ) ;
#18683 = CARTESIAN_POINT ( 'NONE',  ( -10.04416526290807710, -25.50457296725819489, 32.04492750791695954 ) ) ;
#18684 = LINE ( 'NONE', #10825, #17674 ) ;
#18685 = VECTOR ( 'NONE', #14827, 999.9999999999998863 ) ;
#18686 = CARTESIAN_POINT ( 'NONE',  ( -12.35725562635143682, -19.75228648362908501, 36.20117750791695954 ) ) ;
#18687 = DIRECTION ( 'NONE',  ( -0.000000000000000000, -1.000000000000000000, -0.000000000000000000 ) ) ;
#18688 = CARTESIAN_POINT ( 'NONE',  ( -11.21908421996106142, -27.53959229564982181, 29.20507249208304046 ) ) ;
#18689 = VECTOR ( 'NONE', #12948, 1000.000000000000114 ) ;
#18690 = CARTESIAN_POINT ( 'NONE',  ( 1.767766952966369987, 65.76776695296638309, 48.89999999999999858 ) ) ;
#18691 = DIRECTION ( 'NONE',  ( 0.000000000000000000, -1.000000000000000000, 0.000000000000000000 ) ) ;
#18692 = DIRECTION ( 'NONE',  ( 0.000000000000000000, 0.000000000000000000, 1.000000000000000000 ) ) ;
#18693 = CARTESIAN_POINT ( 'NONE',  ( 4.592425496802577917E-16, 61.50000000000000000, 48.59999999999999432 ) ) ;
#18694 = CARTESIAN_POINT ( 'NONE',  ( -7.999999999999986677, 68.00000000000000000, 45.00000000000000000 ) ) ;
#18695 = ORIENTED_EDGE ( 'NONE', *, *, #11623, .F. ) ;
#18696 = SURFACE_STYLE_FILL_AREA ( #18601 ) ;
#18697 = VECTOR ( 'NONE', #16830, 1000.000000000000000 ) ;
#18698 = DIRECTION ( 'NONE',  ( 0.000000000000000000, 0.000000000000000000, 1.000000000000000000 ) ) ;
#18699 = CARTESIAN_POINT ( 'NONE',  ( -16.64274437364856496, -26.51566270880199738, 28.32617750791696665 ) ) ;
#18700 = CARTESIAN_POINT ( 'NONE',  ( -24.00000000000000000, 53.00000000000000711, -6.000000000000005329 ) ) ;
#18701 = CARTESIAN_POINT ( 'NONE',  ( -20.97976432393974022, -27.64274437364858628, 30.73632249208304046 ) ) ;
#18702 = CARTESIAN_POINT ( 'NONE',  ( -2.066987300000001859, 64.85617417291294373, 45.50000000109247367 ) ) ;
#18703 = ORIENTED_EDGE ( 'NONE', *, *, #5467, .F. ) ;
#18704 = CARTESIAN_POINT ( 'NONE',  ( 1.844224359752661968, -41.39960408384398249, 1.500000000000000000 ) ) ;
#18705 = CARTESIAN_POINT ( 'NONE',  ( 2.500000000000001776, 64.00000000000000000, 45.70000000218494307 ) ) ;
#18706 = CARTESIAN_POINT ( 'NONE',  ( -1.461580736456473462, 62.53841926354353120, 46.45000000109246940 ) ) ;
#18707 = LINE ( 'NONE', #670, #612 ) ;
#18708 = CARTESIAN_POINT ( 'NONE',  ( 0.000000000000000000, 1.478016689125442484, -1.626303258728256651E-15 ) ) ;
#18709 = LINE ( 'NONE', #9945, #8779 ) ;
#18710 = FACE_OUTER_BOUND ( 'NONE', #18519, .T. ) ;
#18711 = VERTEX_POINT ( 'NONE', #3057 ) ;
#18712 = EDGE_LOOP ( 'NONE', ( #14040, #2760 ) ) ;
#18713 = CARTESIAN_POINT ( 'NONE',  ( -17.04047135212043784, -30.95583473709190159, 33.35742750791695244 ) ) ;
#18714 = ORIENTED_EDGE ( 'NONE', *, *, #12508, .F. ) ;
#18716 = VERTEX_POINT ( 'NONE', #10400 ) ;
#18715 = ORIENTED_EDGE ( 'NONE', *, *, #15601, .F. ) ;
#18717 = CARTESIAN_POINT ( 'NONE',  ( -12.92450931948790149, -21.68318583509881137, 33.14257249208304756 ) ) ;
#18718 = CARTESIAN_POINT ( 'NONE',  ( -21.95583473709191580, -21.95952864787954084, 34.66992750791696665 ) ) ;
#18719 = FACE_OUTER_BOUND ( 'NONE', #389, .T. ) ;
#18720 = CARTESIAN_POINT ( 'NONE',  ( 1.035533905932739751, 61.50000000000000000, 47.95000000218495018 ) ) ;
#18721 = CARTESIAN_POINT ( 'NONE',  ( 4.189131392896579875, 32.57932772728315740, 53.90500129688597042 ) ) ;
#18722 = VERTEX_POINT ( 'NONE', #16494 ) ;
#18723 = CARTESIAN_POINT ( 'NONE',  ( -17.51566270880201159, -22.35725562635141728, 24.38867750791696665 ) ) ;
#18724 = ADVANCED_FACE ( 'NONE', ( #10296 ), #17869, .T. ) ;
#18725 = DIRECTION ( 'NONE',  ( 0.000000000000000000, 0.000000000000000000, -1.000000000000000000 ) ) ;
#18726 = ORIENTED_EDGE ( 'NONE', *, *, #7988, .T. ) ;
#18727 = DIRECTION ( 'NONE',  ( -0.000000000000000000, -0.000000000000000000, -1.000000000000000000 ) ) ;
#18728 = EDGE_LOOP ( 'NONE', ( #212, #1170, #11464, #18109 ) ) ;
#18729 = CARTESIAN_POINT ( 'NONE',  ( -3.065533689247737392, -43.60761626555502346, 3.000000000000000000 ) ) ;
#18730 =( REPRESENTATION_RELATIONSHIP ('NONE','NONE', #7912, #15417 ) REPRESENTATION_RELATIONSHIP_WITH_TRANSFORMATION ( #18357 )SHAPE_REPRESENTATION_RELATIONSHIP( ) );
#18731 = FACE_OUTER_BOUND ( 'NONE', #18548, .T. ) ;
#18732 = DIRECTION ( 'NONE',  ( 0.000000000000000000, 0.000000000000000000, -1.000000000000000000 ) ) ;
#18733 = CARTESIAN_POINT ( 'NONE',  ( -0.8561741729129465073, 61.93301270000000613, 46.50000000109247367 ) ) ;
#18734 = CARTESIAN_POINT ( 'NONE',  ( 3.796994071234847710E-16, 61.93301269999999903, 47.55000000109247082 ) ) ;
#18735 = CARTESIAN_POINT ( 'NONE',  ( -50.00000000000002132, 3.000000000000000000, -60.00000000000002132 ) ) ;
#18736 = DIRECTION ( 'NONE',  ( 0.000000000000000000, 0.000000000000000000, -1.000000000000000000 ) ) ;
#18737 = FACE_OUTER_BOUND ( 'NONE', #893, .T. ) ;
#18738 = ORIENTED_EDGE ( 'NONE', *, *, #5181, .F. ) ;
#18739 = VERTEX_POINT ( 'NONE', #14725 ) ;
#18740 = CARTESIAN_POINT ( 'NONE',  ( -9.955834737091912245, -22.82508104294696594, 36.85742750791696665 ) ) ;
#18741 = DIRECTION ( 'NONE',  ( 0.000000000000000000, 0.7071067811865494601, -0.7071067811865455743 ) ) ;
#18742 = ADVANCED_FACE ( 'NONE', ( #4442 ), #15124, .F. ) ;
#18743 = ORIENTED_EDGE ( 'NONE', *, *, #4629, .T. ) ;
#18744 = EDGE_CURVE ( 'NONE', #6113, #2052, #5905, .T. ) ;
#18745 = CARTESIAN_POINT ( 'NONE',  ( -9.955834737091903364, -25.17491895705294880, 34.01757249208303335 ) ) ;
#18746 = EDGE_CURVE ( 'NONE', #11621, #13466, #7573, .T. ) ;
#18747 = CARTESIAN_POINT ( 'NONE',  ( -41.00000000000000711, 53.00000000000000711, -37.50000000000000711 ) ) ;
#18748 = CARTESIAN_POINT ( 'NONE',  ( -14.36097942780925685, -20.95583473709189093, 37.95507249208304046 ) ) ;
#18749 = ORIENTED_EDGE ( 'NONE', *, *, #3755, .F. ) ;
#18750 = CARTESIAN_POINT ( 'NONE',  ( -2.500000000000006661, 65.03553390593272354, 46.85000000218494165 ) ) ;
#18751 = ORIENTED_EDGE ( 'NONE', *, *, #3395, .F. ) ;
#18752 = PLANE ( 'NONE',  #7839 ) ;
#18753 = FACE_OUTER_BOUND ( 'NONE', #13343, .T. ) ;
#18754 = CARTESIAN_POINT ( 'NONE',  ( -24.00000000000000711, 110.0000000000000000, 27.50000000000000000 ) ) ;
#18755 = FACE_OUTER_BOUND ( 'NONE', #13625, .T. ) ;
#18756 = FACE_BOUND ( 'NONE', #196, .T. ) ;
#18757 = AXIS2_PLACEMENT_3D ( 'NONE', #14215, #782, #6767 ) ;
#18758 = FACE_OUTER_BOUND ( 'NONE', #9233, .T. ) ;
#18759 = EDGE_CURVE ( 'NONE', #2559, #1624, #16591, .T. ) ;
#18760 = ORIENTED_EDGE ( 'NONE', *, *, #4645, .F. ) ;
#18761 = VECTOR ( 'NONE', #1532, 1000.000000000000000 ) ;
#18762 = CARTESIAN_POINT ( 'NONE',  ( -9.999999999999994671, -24.16482700510257686, 26.57617750791695954 ) ) ;
#18763 = CARTESIAN_POINT ( 'NONE',  ( 2.066987300000002303, 63.14382582708705627, 47.50000000109246656 ) ) ;
#18764 = CARTESIAN_POINT ( 'NONE',  ( -10.04416526290808953, -22.49542703274172695, 38.83007249208302625 ) ) ;
#18765 = CARTESIAN_POINT ( 'NONE',  ( 3.399999999999996803, 29.47747564417430155, 56.65425233947098604 ) ) ;
#18766 = CARTESIAN_POINT ( 'NONE',  ( -20.04416526290808065, -25.17491895705300209, 28.98242750791695244 ) ) ;
#18767 = DIRECTION ( 'NONE',  ( -1.000000000000000000, 0.000000000000000000, -0.000000000000000000 ) ) ;
#18769 = CARTESIAN_POINT ( 'NONE',  ( -20.04416526290808065, -25.17491895705300209, 39.48242750791695244 ) ) ;
#18768 = VECTOR ( 'NONE', #5887, 1000.000000000000000 ) ;
#18770 = PLANE ( 'NONE',  #17805 ) ;
#18771 = CARTESIAN_POINT ( 'NONE',  ( -18.53959229564983247, -27.78091578003891016, 20.01757249208304046 ) ) ;
#18772 = CARTESIAN_POINT ( 'NONE',  ( 1.767766952966370653, 62.23223304703363112, 48.69999999999999574 ) ) ;
#18773 = CARTESIAN_POINT ( 'NONE',  ( -10.00000000000000000, -0.000000000000000000, 30.00000000000000000 ) ) ;
#18774 = VECTOR ( 'NONE', #14143, 1000.000000000000000 ) ;
#18775 = VECTOR ( 'NONE', #383, 1000.000000000000000 ) ;
#18776 = EDGE_CURVE ( 'NONE', #4687, #8924, #8965, .T. ) ;
#18777 = DIRECTION ( 'NONE',  ( -0.7071067811865312525, 0.000000000000000000, 0.7071067811865637820 ) ) ;
#18778 = CARTESIAN_POINT ( 'NONE',  ( -2.500000000000001776, 65.03553390593273775, 48.35000000000000142 ) ) ;
#18779 = CARTESIAN_POINT ( 'NONE',  ( -24.00000000000000000, 53.00000000000000711, 13.49999999999999822 ) ) ;
#18780 = AXIS2_PLACEMENT_3D ( 'NONE', #17949, #13619, #204 ) ;
#18781 = ORIENTED_EDGE ( 'NONE', *, *, #12291, .T. ) ;
#18782 = CARTESIAN_POINT ( 'NONE',  ( -1.265664690411616068E-16, 66.06698730000000808, 46.15000000109247225 ) ) ;
#18783 = CARTESIAN_POINT ( 'NONE',  ( -13.49542703274178379, -19.04416526290806289, -0.7675724920830416798 ) ) ;
#18784 = ADVANCED_FACE ( 'NONE', ( #11773 ), #16289, .T. ) ;
#18785 = DIRECTION ( 'NONE',  ( 0.000000000000000000, -1.000000000000000000, 0.000000000000000000 ) ) ;
#18786 = CARTESIAN_POINT ( 'NONE',  ( -12.95952864787948755, -30.95583473709188382, 40.14257249208304756 ) ) ;
#18787 = AXIS2_PLACEMENT_3D ( 'NONE', #18819, #970, #11349 ) ;
#18788 = CARTESIAN_POINT ( 'NONE',  ( -2.066987300000001415, 64.00000000000000000, 49.75000000109246656 ) ) ;
#18789 = ORIENTED_EDGE ( 'NONE', *, *, #18302, .T. ) ;
#18790 = LINE ( 'NONE', #6824, #18490 ) ;
#18791 = LINE ( 'NONE', #2504, #15074 ) ;
#18792 = AXIS2_PLACEMENT_3D ( 'NONE', #13050, #18954, #16104 ) ;
#18793 = CARTESIAN_POINT ( 'NONE',  ( 0.8561741729129460632, 66.06698730000000808, 45.30000000109246372 ) ) ;
#18794 = CARTESIAN_POINT ( 'NONE',  ( -25.00000000000001421, 0.000000000000000000, 47.49999999999997868 ) ) ;
#18795 = DIRECTION ( 'NONE',  ( 1.000000000000000000, 0.000000000000000000, 0.000000000000000000 ) ) ;
#18796 = EDGE_CURVE ( 'NONE', #8886, #15578, #2695, .T. ) ;
#18797 = CARTESIAN_POINT ( 'NONE',  ( -2.750000000000020872, 118.0000000000000142, 40.49999999999995737 ) ) ;
#18798 = AXIS2_PLACEMENT_3D ( 'NONE', #2441, #9795, #8612 ) ;
#18799 = ADVANCED_BREP_SHAPE_REPRESENTATION ( '', ( #16536, #1791 ), #11098 ) ;
#18800 = CARTESIAN_POINT ( 'NONE',  ( 2.499999999999996891, 62.96446609406726225, 47.94999999999998863 ) ) ;
#18801 = VERTEX_POINT ( 'NONE', #6501 ) ;
#18802 = ORIENTED_EDGE ( 'NONE', *, *, #16305, .T. ) ;
#18803 = CARTESIAN_POINT ( 'NONE',  ( -9.996306089212408708, -18.75498260482328661, 6.892572492083038682 ) ) ;
#18804 = EDGE_LOOP ( 'NONE', ( #11840, #16156, #3350, #1670 ) ) ;
#18805 = PRESENTATION_LAYER_ASSIGNMENT (  '', '', ( #18516 ) ) ;
#18807 = VERTEX_POINT ( 'NONE', #12568 ) ;
#18806 = EDGE_LOOP ( 'NONE', ( #15360, #8552 ) ) ;
#18808 = PRODUCT ( 'spring', 'spring', '', ( #5899 ) ) ;
#18809 = CARTESIAN_POINT ( 'NONE',  ( -18.04416526290808775, -23.36097942780924441, 26.14257249208303691 ) ) ;
#18810 = CARTESIAN_POINT ( 'NONE',  ( -9.754982604823348780, -18.99630608921234654, 31.16992750791695954 ) ) ;
#18811 = AXIS2_PLACEMENT_3D ( 'NONE', #1412, #13454, #4761 ) ;
#18812 = FACE_BOUND ( 'NONE', #2724, .T. ) ;
#18813 = CARTESIAN_POINT ( 'NONE',  ( 1.767766952966370653, 62.23223304703363112, 48.00000000218494023 ) ) ;
#18814 = CARTESIAN_POINT ( 'NONE',  ( -2.500000000000001776, 64.00000000000000000, 49.30000000218494449 ) ) ;
#18815 = ORIENTED_EDGE ( 'NONE', *, *, #5328, .T. ) ;
#18816 = AXIS2_PLACEMENT_3D ( 'NONE', #850, #6830, #7117 ) ;
#18817 = LINE ( 'NONE', #2530, #14419 ) ;
#18818 = ORIENTED_EDGE ( 'NONE', *, *, #18941, .F. ) ;
#18819 = CARTESIAN_POINT ( 'NONE',  ( -45.00000000000000000, 3.000000000000000000, 54.99999999999998579 ) ) ;
#18820 = ORIENTED_EDGE ( 'NONE', *, *, #7198, .T. ) ;
#18821 = CARTESIAN_POINT ( 'NONE',  ( 2.500000000000001776, 64.00000000000000000, 47.19999999999999574 ) ) ;
#18822 = FACE_OUTER_BOUND ( 'NONE', #2871, .T. ) ;
#18823 = DIRECTION ( 'NONE',  ( -0.000000000000000000, 1.000000000000000000, -0.000000000000000000 ) ) ;
#18824 = CARTESIAN_POINT ( 'NONE',  ( -2.066987300000001859, 64.85617417291294373, 45.50000000109247367 ) ) ;
#18825 = VECTOR ( 'NONE', #16155, 1000.000000000000000 ) ;
#18826 = CARTESIAN_POINT ( 'NONE',  ( -7.499999999999994671, -38.00000000000000000, 4.500000000000000888 ) ) ;
#18827 = VECTOR ( 'NONE', #6002, 1000.000000000000000 ) ;
#18828 = CARTESIAN_POINT ( 'NONE',  ( 2.500000000000002220, 62.96446609406726225, 47.25000000218494023 ) ) ;
#18829 = LINE ( 'NONE', #705, #15214 ) ;
#18830 = ORIENTED_EDGE ( 'NONE', *, *, #18744, .F. ) ;
#18831 = ORIENTED_EDGE ( 'NONE', *, *, #14964, .T. ) ;
#18832 = EDGE_CURVE ( 'NONE', #2052, #5165, #9429, .T. ) ;
#18834 = EDGE_CURVE ( 'NONE', #13602, #2358, #3363, .T. ) ;
#18833 = CARTESIAN_POINT ( 'NONE',  ( -7.999999999999996447, -24.16482700510256976, 5.576177507916956877 ) ) ;
#18835 = VECTOR ( 'NONE', #497, 1000.000000000000000 ) ;
#18836 = CARTESIAN_POINT ( 'NONE',  ( -41.00000000000000711, 110.0000000000000000, 8.000000000000000000 ) ) ;
#18837 = EDGE_LOOP ( 'NONE', ( #18011, #11783, #6181, #556 ) ) ;
#18838 = CARTESIAN_POINT ( 'NONE',  ( -12.35725562635140307, -28.24771351637085459, 34.67382249208304046 ) ) ;
#18839 = EDGE_CURVE ( 'NONE', #14325, #5967, #10893, .T. ) ;
#18840 = PLANE ( 'NONE',  #5611 ) ;
#18841 = APPLICATION_CONTEXT ( 'automotive_design' ) ;
#18842 = EDGE_LOOP ( 'NONE', ( #6849, #13219, #3343, #8918 ) ) ;
#18843 = CARTESIAN_POINT ( 'NONE',  ( -11.95583473709190514, -24.63902057219072361, 34.01757249208304046 ) ) ;
#18844 = LINE ( 'NONE', #11275, #17259 ) ;
#18845 = ORIENTED_EDGE ( 'NONE', *, *, #6958, .T. ) ;
#18846 = AXIS2_PLACEMENT_3D ( 'NONE', #1729, #10834, #255 ) ;
#18847 = LINE ( 'NONE', #8539, #13112 ) ;
#18848 = ORIENTED_EDGE ( 'NONE', *, *, #965, .T. ) ;
#18849 = FACE_OUTER_BOUND ( 'NONE', #330, .T. ) ;
#18850 = FACE_OUTER_BOUND ( 'NONE', #12834, .T. ) ;
#18851 = CIRCLE ( 'NONE', #7580, 2.055000000000000160 ) ;
#18852 = CARTESIAN_POINT ( 'NONE',  ( 44.99999999999998579, 3.000000000000000000, -56.49999999999998579 ) ) ;
#18853 = EDGE_CURVE ( 'NONE', #9106, #17089, #3553, .T. ) ;
#18854 = EDGE_CURVE ( 'NONE', #17823, #2170, #18368, .T. ) ;
#18855 = EDGE_CURVE ( 'NONE', #13224, #2362, #16888, .T. ) ;
#18856 = CARTESIAN_POINT ( 'NONE',  ( -10.04416526290807710, -25.50457296725819489, 32.04492750791695954 ) ) ;
#18857 = LINE ( 'NONE', #5239, #12344 ) ;
#18858 = FACE_OUTER_BOUND ( 'NONE', #14534, .T. ) ;
#18859 = FACE_OUTER_BOUND ( 'NONE', #5769, .T. ) ;
#18860 = DIRECTION ( 'NONE',  ( 3.493455720571401687E-15, 0.7071067811865496822, -0.7071067811865454633 ) ) ;
#18861 = ORIENTED_EDGE ( 'NONE', *, *, #13459, .T. ) ;
#18862 = ADVANCED_FACE ( 'NONE', ( #16994, #13939 ), #3454, .T. ) ;
#18863 = ORIENTED_EDGE ( 'NONE', *, *, #6865, .T. ) ;
#18864 = AXIS2_PLACEMENT_3D ( 'NONE', #15248, #18682, #1818 ) ;
#18865 = CARTESIAN_POINT ( 'NONE',  ( -16.17491895705301275, -18.95583473709189803, 35.54492750791695954 ) ) ;
#18866 = CARTESIAN_POINT ( 'NONE',  ( 0.8561741729129460632, 66.06698729999999387, 49.30000000109246372 ) ) ;
#18867 = CARTESIAN_POINT ( 'NONE',  ( -10.58745947852648328, -26.35725562635138530, 34.23632249208304046 ) ) ;
#18868 = CYLINDRICAL_SURFACE ( 'NONE', #5962, 2.499999999999998668 ) ;
#18869 = CARTESIAN_POINT ( 'NONE',  ( 1.767766952966370653, 62.23223304703363112, 46.40000000218494591 ) ) ;
#18870 = CARTESIAN_POINT ( 'NONE',  ( -19.41254052147348830, -26.35725562635142083, 34.01367750791696665 ) ) ;
#18871 = CARTESIAN_POINT ( 'NONE',  ( -10.00000000000000000, -32.50000000000000711, -3.000000000000000000 ) ) ;
#18872 = CARTESIAN_POINT ( 'NONE',  ( -16.17491895705301275, -18.95583473709189448, 30.29492750791695954 ) ) ;
#18873 = DIRECTION ( 'NONE',  ( 0.9863224920830413467, 5.275954983314436132E-15, 0.1648270051026190230 ) ) ;
#18874 = CARTESIAN_POINT ( 'NONE',  ( -19.99999999999999645, -24.16482700510261949, 36.42382249208304046 ) ) ;
#18875 = EDGE_CURVE ( 'NONE', #10175, #12225, #709, .T. ) ;
#18876 = ADVANCED_FACE ( 'NONE', ( #2172 ), #15423, .F. ) ;
#18877 = CARTESIAN_POINT ( 'NONE',  ( -2.066987300000001415, 63.14382582708705627, 45.00000000109246656 ) ) ;
#18878 = CARTESIAN_POINT ( 'NONE',  ( -0.8561741729129461742, 66.06698730000000808, 49.60000000109247509 ) ) ;
#18879 = CARTESIAN_POINT ( 'NONE',  ( 44.99999999999997158, 3.000000000000000000, 53.50000000000000000 ) ) ;
#18880 = EDGE_CURVE ( 'NONE', #15859, #10068, #14034, .T. ) ;
#18881 = CARTESIAN_POINT ( 'NONE',  ( 2.066987300000001415, 64.00000000000000000, 45.35000000109246798 ) ) ;
#18882 = CARTESIAN_POINT ( 'NONE',  ( 3.000000000000002665, 3.367778697655221012E-16, -2.750000000000000000 ) ) ;
#18883 = B_SPLINE_CURVE_WITH_KNOTS ( 'NONE', 3,
 ( #16391, #4738, #11968, #9135 ),
 .UNSPECIFIED., .F., .F.,
 ( 4, 4 ),
 ( 0.000000000000000000, 1.000000000000000000 ),
 .UNSPECIFIED. ) ;
#18884 = ORIENTED_EDGE ( 'NONE', *, *, #16077, .F. ) ;
#18885 = DIRECTION ( 'NONE',  ( 1.000000000000000000, 0.000000000000000000, 0.000000000000000000 ) ) ;
#18886 = CARTESIAN_POINT ( 'NONE',  ( -10.75228648362910100, -26.64274437364854009, 0.7636775079169582092 ) ) ;
#18887 = CARTESIAN_POINT ( 'NONE',  ( 2.499999999999996003, 65.03553390593275196, 48.85000000000000142 ) ) ;
#18888 = CARTESIAN_POINT ( 'NONE',  ( -12.95952864787948755, -30.95583473709188382, 34.89257249208303335 ) ) ;
#18889 = CARTESIAN_POINT ( 'NONE',  ( -1.461580736456473906, 65.46158073645646880, 48.85000000109246798 ) ) ;
#18890 = EDGE_CURVE ( 'NONE', #15274, #2308, #12462, .T. ) ;
#18891 = VERTEX_POINT ( 'NONE', #15314 ) ;
#18892 = DIRECTION ( 'NONE',  ( 0.000000000000000000, 1.000000000000000000, 0.000000000000000000 ) ) ;
#18893 = DIRECTION ( 'NONE',  ( 0.000000000000000000, -0.7071067811865492381, 0.7071067811865457964 ) ) ;
#18894 = CARTESIAN_POINT ( 'NONE',  ( -0.8561741729129466183, 61.93301270000000613, 46.50000000109247367 ) ) ;
#18895 = CARTESIAN_POINT ( 'NONE',  ( 44.99999999999998579, 3.000000000000000000, -54.99999999999998579 ) ) ;
#18896 = CARTESIAN_POINT ( 'NONE',  ( -41.00000000000000711, 53.00000000000000711, 6.999999999999999112 ) ) ;
#18897 = LINE ( 'NONE', #6659, #14911 ) ;
#18898 = ORIENTED_EDGE ( 'NONE', *, *, #4029, .T. ) ;
#18899 = VERTEX_POINT ( 'NONE', #4839 ) ;
#18900 = CARTESIAN_POINT ( 'NONE',  ( -11.64274437364854187, -30.14459132904234195, 37.95117750791695244 ) ) ;
#18901 = ORIENTED_EDGE ( 'NONE', *, *, #888, .T. ) ;
#18903 = ORIENTED_EDGE ( 'NONE', *, *, #2641, .F. ) ;
#18902 = ORIENTED_EDGE ( 'NONE', *, *, #18796, .F. ) ;
#18904 = CARTESIAN_POINT ( 'NONE',  ( -11.95583473709191047, -23.36097942780921954, 5.357427507916959541 ) ) ;
#18905 = CARTESIAN_POINT ( 'NONE',  ( -13.28918265808472299, -31.04416526290805933, 32.91992750791695244 ) ) ;
#18906 = CARTESIAN_POINT ( 'NONE',  ( 2.500000000000000000, 2.357898499370431722, -2.818925648462311528E-15 ) ) ;
#18907 = CARTESIAN_POINT ( 'NONE',  ( -1.530808498934192803E-16, 66.50000000000000000, 47.50000000218494023 ) ) ;
#18908 = DIRECTION ( 'NONE',  ( -1.000000000000000000, -0.000000000000000000, -0.000000000000000000 ) ) ;
#18909 = ORIENTED_EDGE ( 'NONE', *, *, #16580, .T. ) ;
#18910 = CARTESIAN_POINT ( 'NONE',  ( -32.50000000000000000, 52.00000000000000711, -35.00000000000000000 ) ) ;
#18911 = ORIENTED_EDGE ( 'NONE', *, *, #19018, .T. ) ;
#18912 = CARTESIAN_POINT ( 'NONE',  ( 2.500000000000000000, -1.178949249685214307, 2.042000000000002036 ) ) ;
#18913 = VERTEX_POINT ( 'NONE', #10793 ) ;
#18914 = PLANE ( 'NONE',  #17580 ) ;
#18915 = FACE_BOUND ( 'NONE', #17573, .T. ) ;
#18916 = FACE_OUTER_BOUND ( 'NONE', #10671, .T. ) ;
#18917 = CARTESIAN_POINT ( 'NONE',  ( 2.066987300000002303, 63.14382582708705627, 49.30000000109246372 ) ) ;
#18918 = CARTESIAN_POINT ( 'NONE',  ( -7.999999999999996447, -32.00000000000000711, 1.500000000000000000 ) ) ;
#18919 = CARTESIAN_POINT ( 'NONE',  ( 1.767766952966370653, 62.23223304703363112, 49.49999999999999289 ) ) ;
#18920 = DIRECTION ( 'NONE',  ( -0.000000000000000000, -0.000000000000000000, -1.000000000000000000 ) ) ;
#18921 = ORIENTED_EDGE ( 'NONE', *, *, #1811, .F. ) ;
#18922 = VERTEX_POINT ( 'NONE', #5030 ) ;
#18923 = CARTESIAN_POINT ( 'NONE',  ( -17.35725562635144215, -19.58745947852648683, 40.57617750791696665 ) ) ;
#18924 = DIRECTION ( 'NONE',  ( -7.709882115452476934E-17, -0.000000000000000000, -1.000000000000000000 ) ) ;
#18925 = ORIENTED_EDGE ( 'NONE', *, *, #11807, .F. ) ;
#18926 = VECTOR ( 'NONE', #238, 1000.000000000000000 ) ;
#18927 = CARTESIAN_POINT ( 'NONE',  ( -13.35725562635141195, -26.51566270880198672, 8.423822492083042235 ) ) ;
#18928 = CARTESIAN_POINT ( 'NONE',  ( 46.99999999999998579, 30.00000000000000355, 37.49999999999996447 ) ) ;
#18929 = ORIENTED_EDGE ( 'NONE', *, *, #10203, .F. ) ;
#18930 = CARTESIAN_POINT ( 'NONE',  ( -17.07549068051208963, -26.31681416490115311, 35.76757249208304756 ) ) ;
#18931 = CARTESIAN_POINT ( 'NONE',  ( -41.00000000000000711, 110.0000000000000000, -12.50000000000000000 ) ) ;
#18932 = EDGE_LOOP ( 'NONE', ( #1240, #3995 ) ) ;
#18933 = CARTESIAN_POINT ( 'NONE',  ( 1.767766952966369987, 65.76776695296638309, 46.60000000218494165 ) ) ;
#18934 = ORIENTED_EDGE ( 'NONE', *, *, #16240, .F. ) ;
#18935 = DIRECTION ( 'NONE',  ( 0.000000000000000000, 0.4999999999999991673, -0.8660254037844391517 ) ) ;
#18936 = EDGE_CURVE ( 'NONE', #17652, #982, #16161, .T. ) ;
#18937 = LINE ( 'NONE', #11564, #9852 ) ;
#18938 = AXIS2_PLACEMENT_3D ( 'NONE', #10816, #16813, #243 ) ;
#18939 = VECTOR ( 'NONE', #37, 1000.000000000000000 ) ;
#18940 = DIRECTION ( 'NONE',  ( 0.000000000000000000, 0.000000000000000000, -1.000000000000000000 ) ) ;
#18941 = EDGE_CURVE ( 'NONE', #3686, #9430, #6404, .T. ) ;
#18942 = CARTESIAN_POINT ( 'NONE',  ( -10.04416526290807710, -25.50457296725819489, 21.54492750791695599 ) ) ;
#18943 = DIRECTION ( 'NONE',  ( -1.000000000000000000, -0.000000000000000000, -0.000000000000000000 ) ) ;
#18944 = FACE_OUTER_BOUND ( 'NONE', #9300, .T. ) ;
#18946 = EDGE_CURVE ( 'NONE', #18251, #11634, #8161, .T. ) ;
#18945 = CARTESIAN_POINT ( 'NONE',  ( -11.46040770435012668, -27.78091578003887463, 0.9824275079169582092 ) ) ;
#18947 = CARTESIAN_POINT ( 'NONE',  ( -45.00000000000000000, -1.285879139104706187E-16, 53.39999999999999147 ) ) ;
#18948 = VERTEX_POINT ( 'NONE', #604 ) ;
#18949 = CARTESIAN_POINT ( 'NONE',  ( -19.95583473709190514, -25.50457296725822687, 4.705072492083039570 ) ) ;
#18950 = AXIS2_PLACEMENT_3D ( 'NONE', #14623, #16491, #2859 ) ;
#18951 = CARTESIAN_POINT ( 'NONE',  ( -10.04416526290807710, -25.50457296725819489, 37.29492750791697375 ) ) ;
#18952 = CARTESIAN_POINT ( 'NONE',  ( -2.066987300000001415, 64.00000000000000000, 49.55000000109247082 ) ) ;
#18953 = CARTESIAN_POINT ( 'NONE',  ( -13.82508104294702100, -18.95583473709188382, 32.70507249208304046 ) ) ;
#18954 = DIRECTION ( 'NONE',  ( -1.000000000000000000, -0.000000000000000000, -0.000000000000000000 ) ) ;
#18955 = ORIENTED_EDGE ( 'NONE', *, *, #8403, .F. ) ;
#18956 = DIRECTION ( 'NONE',  ( -0.000000000000000000, -0.000000000000000000, -1.000000000000000000 ) ) ;
#18957 = CARTESIAN_POINT ( 'NONE',  ( -16.50457296725820555, -28.95583473709189448, 28.10742750791695954 ) ) ;
#18958 = EDGE_CURVE ( 'NONE', #17064, #6956, #6597, .T. ) ;
#18959 = LINE ( 'NONE', #19156, #145 ) ;
#18960 = CARTESIAN_POINT ( 'NONE',  ( -18.53959229564986799, -20.21908421996107563, 40.35742750791695954 ) ) ;
#18961 = CARTESIAN_POINT ( 'NONE',  ( -41.00000000000000000, 52.00000000000000711, 30.00000000000000000 ) ) ;
#18962 = CARTESIAN_POINT ( 'NONE',  ( -18.53959229564983247, -27.78091578003891016, 41.01757249208303335 ) ) ;
#18963 = CARTESIAN_POINT ( 'NONE',  ( 3.796994071234847710E-16, 61.93301269999999903, 45.15000000109247225 ) ) ;
#18964 = CARTESIAN_POINT ( 'NONE',  ( 1.461580736456473684, 65.46158073645646880, 48.65000000109247225 ) ) ;
#18965 = VECTOR ( 'NONE', #8551, 1000.000000000000000 ) ;
#18966 = VECTOR ( 'NONE', #13680, 1000.000000000000000 ) ;
#18967 = PRODUCT_DEFINITION_SHAPE ( 'NONE', 'NONE',  #19400 ) ;
#18968 = FACE_OUTER_BOUND ( 'NONE', #15982, .T. ) ;
#18969 = CARTESIAN_POINT ( 'NONE',  ( -1.035533905932738863, 61.50000000000000000, 49.35000000000000142 ) ) ;
#18970 = DIRECTION ( 'NONE',  ( 0.000000000000000000, 1.000000000000000000, -0.000000000000000000 ) ) ;
#18971 = ORIENTED_EDGE ( 'NONE', *, *, #10934, .F. ) ;
#18972 = EDGE_CURVE ( 'NONE', #9095, #19310, #13013, .T. ) ;
#18973 = CARTESIAN_POINT ( 'NONE',  ( -2.066987300000001415, 64.85617417291294373, 45.50000000109247367 ) ) ;
#18974 = EDGE_CURVE ( 'NONE', #8044, #1767, #3261, .T. ) ;
#18975 = CARTESIAN_POINT ( 'NONE',  ( -12.64274437364855252, -28.41254052147347053, 6.451177507916959541 ) ) ;
#18976 = CARTESIAN_POINT ( 'NONE',  ( -32.50000000000001421, 0.000000000000000000, 44.99999999999997868 ) ) ;
#18977 = EDGE_CURVE ( 'NONE', #14696, #17240, #5406, .T. ) ;
#18978 = CARTESIAN_POINT ( 'NONE',  ( -13.28918265808478694, -16.95583473709189093, 37.95507249208304046 ) ) ;
#18979 = AXIS2_PLACEMENT_3D ( 'NONE', #2191, #7716, #8185 ) ;
#18980 = AXIS2_PLACEMENT_3D ( 'NONE', #5833, #7194, #13169 ) ;
#18981 = CARTESIAN_POINT ( 'NONE',  ( -1.461580736456473906, 65.46158073645646880, 47.25000000109246656 ) ) ;
#18982 = DIRECTION ( 'NONE',  ( 0.000000000000000000, 1.000000000000000000, 0.000000000000000000 ) ) ;
#18983 = DIRECTION ( 'NONE',  ( 1.000000000000000000, -7.160938508832259686E-15, 7.660538869913580129E-15 ) ) ;
#18984 = CARTESIAN_POINT ( 'NONE',  ( 0.8561741729129460632, 66.06698730000000808, 46.90000000109247225 ) ) ;
#18985 = CARTESIAN_POINT ( 'NONE',  ( 1.300000000000000044, 0.000000000000000000, 0.000000000000000000 ) ) ;
#18986 = FACE_OUTER_BOUND ( 'NONE', #19200, .T. ) ;
#18987 = DIRECTION ( 'NONE',  ( 0.000000000000000000, 1.000000000000000000, 0.000000000000000000 ) ) ;
#18988 = VECTOR ( 'NONE', #13844, 1000.000000000000000 ) ;
#18989 = VECTOR ( 'NONE', #12160, 1000.000000000000000 ) ;
#18990 = CARTESIAN_POINT ( 'NONE',  ( 49.99999999999998579, 3.000000000000000000, 59.99999999999997868 ) ) ;
#18991 = EDGE_CURVE ( 'NONE', #10947, #10091, #16074, .T. ) ;
#18992 = ORIENTED_EDGE ( 'NONE', *, *, #6763, .F. ) ;
#18993 = ORIENTED_EDGE ( 'NONE', *, *, #15404, .T. ) ;
#18994 = EDGE_CURVE ( 'NONE', #6595, #5928, #5529, .T. ) ;
#18995 = CARTESIAN_POINT ( 'NONE',  ( -20.00369391078762860, -18.75498260482333279, 40.35742750791695954 ) ) ;
#18996 = FILL_AREA_STYLE ('',( #952 ) ) ;
#18997 = ORIENTED_EDGE ( 'NONE', *, *, #11373, .F. ) ;
#18999 = VERTEX_POINT ( 'NONE', #6862 ) ;
#18998 = VERTEX_POINT ( 'NONE', #18836 ) ;
#19000 = CARTESIAN_POINT ( 'NONE',  ( -14.83517299489736985, -26.99999999999998579, 40.36132249208304756 ) ) ;
#19001 = CARTESIAN_POINT ( 'NONE',  ( -7.955834737091916686, -22.28918265808470522, 31.60742750791695244 ) ) ;
#19002 = LINE ( 'NONE', #16054, #15719 ) ;
#19003 = CARTESIAN_POINT ( 'NONE',  ( 2.500000000000001776, 65.03553390593273775, 46.55000000218494449 ) ) ;
#19004 = FACE_OUTER_BOUND ( 'NONE', #11963, .T. ) ;
#19005 = VERTEX_POINT ( 'NONE', #5493 ) ;
#19006 =( BOUNDED_CURVE ( )  B_SPLINE_CURVE ( 2, ( #18380, #13855, #618, #17004, #2095, #719, #7983, #16899, #6511 ),
 .UNSPECIFIED., .F., .F. ) 
 B_SPLINE_CURVE_WITH_KNOTS ( ( 3, 2, 2, 2, 3 ),
 ( 0.6428571428571427937, 0.6607142857142855874, 0.6785714285714284921, 0.6964285714285712858, 0.7142857142857141906 ),
 .UNSPECIFIED. ) 
 CURVE ( )  GEOMETRIC_REPRESENTATION_ITEM ( )  RATIONAL_B_SPLINE_CURVE ( ( 1.000000000000000444, 0.9238795325112862944, 1.000000000000000000, 0.9238795325112867385, 1.000000000000000000, 0.9238795325112867385, 1.000000000000000000, 0.9238795325112871826, 0.9999999999999995559 ) ) 
 REPRESENTATION_ITEM ( '' )  );
#19007 = CARTESIAN_POINT ( 'NONE',  ( -41.00000000000000711, 53.00000000000000711, -44.00000000000000000 ) ) ;
#19008 = ORIENTED_EDGE ( 'NONE', *, *, #16407, .F. ) ;
#19009 = LINE ( 'NONE', #18912, #3125 ) ;
#19010 = ORIENTED_EDGE ( 'NONE', *, *, #4719, .T. ) ;
#19011 = CARTESIAN_POINT ( 'NONE',  ( 0.7910017786515960436, 62.09035273295529578, 44.99999999999998579 ) ) ;
#19012 = CARTESIAN_POINT ( 'NONE',  ( 2.500000000000001776, 64.00000000000000000, 49.99999999999999289 ) ) ;
#19013 = FACE_OUTER_BOUND ( 'NONE', #11068, .T. ) ;
#19014 = CARTESIAN_POINT ( 'NONE',  ( -0.8561741729129461742, 66.06698729999999387, 46.20000000109247651 ) ) ;
#19015 = LINE ( 'NONE', #13215, #6287 ) ;
#19016 = CARTESIAN_POINT ( 'NONE',  ( 4.592425496802577917E-16, 61.50000000000000000, 49.39999999999999147 ) ) ;
#19017 = DIRECTION ( 'NONE',  ( -0.000000000000000000, -0.000000000000000000, -1.000000000000000000 ) ) ;
#19018 = EDGE_CURVE ( 'NONE', #869, #5315, #11456, .T. ) ;
#19019 = ORIENTED_EDGE ( 'NONE', *, *, #7932, .F. ) ;
#19021 = ORIENTED_EDGE ( 'NONE', *, *, #148, .F. ) ;
#19020 = ORIENTED_EDGE ( 'NONE', *, *, #12037, .F. ) ;
#19022 = CARTESIAN_POINT ( 'NONE',  ( -15.16482700510259640, -28.99999999999998224, 38.38867750791695954 ) ) ;
#19023 = CARTESIAN_POINT ( 'NONE',  ( -47.00000000000002132, 115.0000000000000000, -60.00000000000002132 ) ) ;
#19024 = ORIENTED_EDGE ( 'NONE', *, *, #12367, .T. ) ;
#19025 = CARTESIAN_POINT ( 'NONE',  ( -18.04416526290808775, -23.36097942780924441, 10.39257249208304223 ) ) ;
#19026 = FACE_OUTER_BOUND ( 'NONE', #17736, .T. ) ;
#19027 = ORIENTED_EDGE ( 'NONE', *, *, #3062, .F. ) ;
#19028 = CARTESIAN_POINT ( 'NONE',  ( -13.35725562635142794, -21.48433729119796709, 4.701177507916959541 ) ) ;
#19029 =( NAMED_UNIT ( * ) SI_UNIT ( $, .STERADIAN. ) SOLID_ANGLE_UNIT ( ) );
#19030 = EDGE_LOOP ( 'NONE', ( #16395, #4723, #4715, #14001 ) ) ;
#19031 = FACE_OUTER_BOUND ( 'NONE', #7761, .T. ) ;
#19032 = ORIENTED_EDGE ( 'NONE', *, *, #11695, .F. ) ;
#19033 = LINE ( 'NONE', #10092, #11283 ) ;
#19034 = CARTESIAN_POINT ( 'NONE',  ( -40.00000000000000711, 113.0000000000000000, -25.49999999999999645 ) ) ;
#19035 = DIRECTION ( 'NONE',  ( 0.000000000000000000, 0.000000000000000000, 1.000000000000000000 ) ) ;
#19036 = CARTESIAN_POINT ( 'NONE',  ( -2.500000000000001776, 64.00000000000000000, 48.50000000218494023 ) ) ;
#19037 = CARTESIAN_POINT ( 'NONE',  ( -19.99999999999999645, -23.83517299489738051, 29.20117750791695599 ) ) ;
#19038 = LINE ( 'NONE', #8548, #7007 ) ;
#19039 = EDGE_CURVE ( 'NONE', #2835, #17031, #17354, .T. ) ;
#19040 = LINE ( 'NONE', #15905, #1775 ) ;
#19041 = ORIENTED_EDGE ( 'NONE', *, *, #2934, .F. ) ;
#19042 = PRODUCT_DEFINITION_CONTEXT ( 'detailed design', #14083, 'design' ) ;
#19043 = CARTESIAN_POINT ( 'NONE',  ( -18.53959229564982536, -27.78091578003890660, 9.517572492083042235 ) ) ;
#19044 = CARTESIAN_POINT ( 'NONE',  ( -15.16482700510258574, -30.99999999999998224, 1.638677507916956433 ) ) ;
#19045 = CARTESIAN_POINT ( 'NONE',  ( -1.265664690411616068E-16, 66.06698730000000808, 46.95000000109246940 ) ) ;
#19046 = CARTESIAN_POINT ( 'NONE',  ( -16.35725562635141372, -26.68048971390461332, 9.298822492083044011 ) ) ;
#19047 = AXIS2_PLACEMENT_3D ( 'NONE', #5348, #19057, #12778 ) ;
#19048 = CARTESIAN_POINT ( 'NONE',  ( 2.500000000000001776, 64.00000000000000000, 48.79999999999999716 ) ) ;
#19049 = ORIENTED_EDGE ( 'NONE', *, *, #6024, .F. ) ;
#19050 = LINE ( 'NONE', #2295, #10942 ) ;
#19051 = CARTESIAN_POINT ( 'NONE',  ( -11.21908421996108629, -20.46040770435011069, 36.41992750791695954 ) ) ;
#19052 = CARTESIAN_POINT ( 'NONE',  ( 2.750000000000009770, 38.00000000000000000, 40.49999999999995737 ) ) ;
#19053 = CARTESIAN_POINT ( 'NONE',  ( 4.999999999999997335, 0.000000000000000000, 0.000000000000000000 ) ) ;
#19054 = DIRECTION ( 'NONE',  ( -0.000000000000000000, -0.000000000000000000, -1.000000000000000000 ) ) ;
#19055 = CARTESIAN_POINT ( 'NONE',  ( -15.16482700510263371, -18.99999999999997868, 42.98632249208304046 ) ) ;
#19056 = CARTESIAN_POINT ( 'NONE',  ( 1.035533905932738197, 66.50000000000000000, 48.14999999999999858 ) ) ;
#19057 = DIRECTION ( 'NONE',  ( 0.000000000000000000, 0.000000000000000000, 1.000000000000000000 ) ) ;
#19058 = CIRCLE ( 'NONE', #3088, 2.999999999999999112 ) ;
#19059 = CARTESIAN_POINT ( 'NONE',  ( 5.800448837981379668, 29.77177811653243822, 56.71286850494553988 ) ) ;
#19060 = CARTESIAN_POINT ( 'NONE',  ( -2.066987300000001415, 63.14382582708705627, 45.00000000109246656 ) ) ;
#19061 = CARTESIAN_POINT ( 'NONE',  ( -40.00000000000000711, 110.0000000000000000, 30.00000000000000000 ) ) ;
#19062 = AXIS2_PLACEMENT_3D ( 'NONE', #8471, #18873, #5627 ) ;
#19063 = ORIENTED_EDGE ( 'NONE', *, *, #9388, .T. ) ;
#19064 = EDGE_CURVE ( 'NONE', #10051, #13646, #9710, .T. ) ;
#19065 = EDGE_CURVE ( 'NONE', #2050, #11844, #15704, .T. ) ;
#19066 = CARTESIAN_POINT ( 'NONE',  ( -10.58745947852649927, -21.64274437364853654, 5.138677507916957765 ) ) ;
#19067 = CARTESIAN_POINT ( 'NONE',  ( -18.78091578003889950, -27.53959229564985378, 7.544927507916956877 ) ) ;
#19068 = DIRECTION ( 'NONE',  ( -1.000000000000000000, 0.000000000000000000, -0.000000000000000000 ) ) ;
#19069 = CARTESIAN_POINT ( 'NONE',  ( -20.00369391078757886, -29.24501739517668142, 35.76757249208303335 ) ) ;
#19070 = AXIS2_PLACEMENT_3D ( 'NONE', #5771, #1663, #19302 ) ;
#19071 = CARTESIAN_POINT ( 'NONE',  ( 0.8561741729129460632, 66.06698729999999387, 47.10000000109246798 ) ) ;
#19072 = CARTESIAN_POINT ( 'NONE',  ( -18.04416526290808420, -24.63902057219074493, 28.98242750791696309 ) ) ;
#19073 = DIRECTION ( 'NONE',  ( 0.000000000000000000, 1.000000000000000000, -0.000000000000000000 ) ) ;
#19074 = AXIS2_PLACEMENT_3D ( 'NONE', #6897, #14250, #820 ) ;
#19075 = CARTESIAN_POINT ( 'NONE',  ( -35.00000000000002132, -6.000000000000000000, -42.50000000000001421 ) ) ;
#19076 = AXIS2_PLACEMENT_3D ( 'NONE', #14686, #10071, #3914 ) ;
#19077 = LINE ( 'NONE', #2798, #19382 ) ;
#19078 = PLANE ( 'NONE',  #6828 ) ;
#19079 = CARTESIAN_POINT ( 'NONE',  ( -24.00000000000000711, 53.00000000000000711, 6.999999999999999112 ) ) ;
#19080 = EDGE_CURVE ( 'NONE', #6552, #15077, #14605, .T. ) ;
#19081 = CARTESIAN_POINT ( 'NONE',  ( 2.066987300000001415, 64.00000000000000000, 47.75000000109246656 ) ) ;
#19082 = LINE ( 'NONE', #12799, #2529 ) ;
#19083 = EDGE_CURVE ( 'NONE', #11529, #1874, #3925, .T. ) ;
#19084 = VECTOR ( 'NONE', #10178, 1000.000000000000000 ) ;
#19085 = CARTESIAN_POINT ( 'NONE',  ( -41.00000000000000711, 53.00000000000000711, -38.50000000000000711 ) ) ;
#19086 = EDGE_LOOP ( 'NONE', ( #3369, #3438 ) ) ;
#19087 = EDGE_LOOP ( 'NONE', ( #12340, #17951, #8116, #3046 ) ) ;
#19088 = APPLICATION_CONTEXT ( 'automotive_design' ) ;
#19089 = CARTESIAN_POINT ( 'NONE',  ( -21.14459132904239169, -20.64274437364858628, 10.61132249208303868 ) ) ;
#19090 = SURFACE_STYLE_USAGE ( .BOTH. , #12017 ) ;
#19091 = VERTEX_POINT ( 'NONE', #14407 ) ;
#19093 = VERTEX_POINT ( 'NONE', #17175 ) ;
#19092 = ORIENTED_EDGE ( 'NONE', *, *, #8903, .F. ) ;
#19094 = CARTESIAN_POINT ( 'NONE',  ( -16.35725562635141372, -26.68048971390461332, 40.79882249208304756 ) ) ;
#19095 = CARTESIAN_POINT ( 'NONE',  ( -9.754982604823348780, -18.99630608921234654, 36.41992750791695954 ) ) ;
#19096 = AXIS2_PLACEMENT_3D ( 'NONE', #19152, #6989, #7180 ) ;
#19097 = DIRECTION ( 'NONE',  ( 0.000000000000000000, -0.8660254037844391517, -0.4999999999999992784 ) ) ;
#19098 = CARTESIAN_POINT ( 'NONE',  ( -1.530808498934192803E-16, 66.50000000000000000, 44.30000000218494449 ) ) ;
#19099 = CYLINDRICAL_SURFACE ( 'NONE', #12813, 1.500000000000001332 ) ;
#19100 = ORIENTED_EDGE ( 'NONE', *, *, #9486, .T. ) ;
#19101 = CARTESIAN_POINT ( 'NONE',  ( 24.00000000000000000, 47.00000000000000711, -67.72004514666936359 ) ) ;
#19102 = ORIENTED_EDGE ( 'NONE', *, *, #15135, .T. ) ;
#19103 = VECTOR ( 'NONE', #18982, 1000.000000000000000 ) ;
#19104 = ORIENTED_EDGE ( 'NONE', *, *, #2927, .F. ) ;
#19105 = CARTESIAN_POINT ( 'NONE',  ( -4.189607678530257395, 32.40336399182267257, 53.72836399182263278 ) ) ;
#19106 = CARTESIAN_POINT ( 'NONE',  ( 34.99999999999999289, -6.000000000000000000, 47.49999999999997868 ) ) ;
#19107 = PLANE ( 'NONE',  #2487 ) ;
#19108 = VECTOR ( 'NONE', #16663, 1000.000000000000000 ) ;
#19109 = CARTESIAN_POINT ( 'NONE',  ( 0.8561741729129472844, 61.93301270000000613, 45.00000000109246656 ) ) ;
#19110 = ADVANCED_FACE ( 'NONE', ( #4126 ), #5589, .F. ) ;
#19111 = CARTESIAN_POINT ( 'NONE',  ( -3.999999999999996447, 47.00000000000000711, 30.00000000000000000 ) ) ;
#19112 = CARTESIAN_POINT ( 'NONE',  ( -1.767766952966369765, 62.23223304703363112, 49.29999999999999716 ) ) ;
#19113 = CARTESIAN_POINT ( 'NONE',  ( -2.500000000000001776, 64.00000000000000000, 47.70000000218494307 ) ) ;
#19114 = ORIENTED_EDGE ( 'NONE', *, *, #11287, .F. ) ;
#19116 = ORIENTED_EDGE ( 'NONE', *, *, #13456, .T. ) ;
#19115 = ORIENTED_EDGE ( 'NONE', *, *, #14948, .T. ) ;
#19117 = EDGE_CURVE ( 'NONE', #3455, #2845, #18067, .T. ) ;
#19118 = CARTESIAN_POINT ( 'NONE',  ( -21.14459132904236327, -27.35725562635143149, 2.513677507916956433 ) ) ;
#19119 = DIRECTION ( 'NONE',  ( -0.000000000000000000, -1.000000000000000000, -0.000000000000000000 ) ) ;
#19120 = VECTOR ( 'NONE', #8925, 1000.000000000000114 ) ;
#19121 = ORIENTED_EDGE ( 'NONE', *, *, #5674, .F. ) ;
#19122 = CARTESIAN_POINT ( 'NONE',  ( -12.68318583509882380, -26.07549068051207541, 8.205072492083042235 ) ) ;
#19123 = AXIS2_PLACEMENT_3D ( 'NONE', #8309, #18987, #15762 ) ;
#19124 = LINE ( 'NONE', #14610, #2480 ) ;
#19125 = VERTEX_POINT ( 'NONE', #12930 ) ;
#19126 = CARTESIAN_POINT ( 'NONE',  ( -14.03132541760401786, -21.04416526290806289, 4.482427507916961318 ) ) ;
#19127 = CARTESIAN_POINT ( 'NONE',  ( 2.499999999999996003, 65.03553390593275196, 48.85000000000000142 ) ) ;
#19128 = VERTEX_POINT ( 'NONE', #3738 ) ;
#19129 = AXIS2_PLACEMENT_3D ( 'NONE', #7453, #4525, #7555 ) ;
#19130 = FACE_OUTER_BOUND ( 'NONE', #6188, .T. ) ;
#19131 = EDGE_LOOP ( 'NONE', ( #7694, #17725, #9059, #10274 ) ) ;
#19132 = ADVANCED_FACE ( 'NONE', ( #2272 ), #14226, .T. ) ;
#19133 = CARTESIAN_POINT ( 'NONE',  ( -40.00000000000000711, 110.0000000000000000, -32.00000000000000000 ) ) ;
#19134 = DIRECTION ( 'NONE',  ( 0.000000000000000000, 0.000000000000000000, -1.000000000000000000 ) ) ;
#19135 = CARTESIAN_POINT ( 'NONE',  ( -1.767766952966369765, 62.23223304703363112, 47.80000000218494449 ) ) ;
#19136 = VECTOR ( 'NONE', #16584, 1000.000000000000000 ) ;
#19137 = PRODUCT_CONTEXT ( 'NONE', #15093, 'mechanical' ) ;
#19138 = DIRECTION ( 'NONE',  ( -0.000000000000000000, -0.000000000000000000, -1.000000000000000000 ) ) ;
#19139 = CARTESIAN_POINT ( 'NONE',  ( -13.82508104294698192, -29.04416526290806644, 22.41992750791695244 ) ) ;
#19140 = LINE ( 'NONE', #17866, #2367 ) ;
#19141 = CARTESIAN_POINT ( 'NONE',  ( -15.16482700510263371, -18.99999999999997868, 0.9863224920830410136 ) ) ;
#19142 = CIRCLE ( 'NONE', #10682, 1.599999999999997202 ) ;
#19143 = LINE ( 'NONE', #15727, #4587 ) ;
#19144 = ORIENTED_EDGE ( 'NONE', *, *, #7485, .F. ) ;
#19145 = CARTESIAN_POINT ( 'NONE',  ( -10.58745947852648328, -26.35725562635138530, 2.736322492083041347 ) ) ;
#19146 = PRODUCT_DEFINITION ( 'UNKNOWN', '', #2978, #13346 ) ;
#19147 = VECTOR ( 'NONE', #3390, 1000.000000000000000 ) ;
#19148 = CARTESIAN_POINT ( 'NONE',  ( -8.855408670957631401, -20.64274437364852943, -0.1113224920830435533 ) ) ;
#19149 = CARTESIAN_POINT ( 'NONE',  ( 2.066987300000002303, 63.14382582708705627, 45.10000000109246798 ) ) ;
#19150 = CARTESIAN_POINT ( 'NONE',  ( -15.96867458239599635, -21.04416526290806999, 6.017572492083043123 ) ) ;
#19151 = AXIS2_PLACEMENT_3D ( 'NONE', #7675, #227, #12174 ) ;
#19152 = CARTESIAN_POINT ( 'NONE',  ( 0.2500000000000002220, 0.000000000000000000, 0.000000000000000000 ) ) ;
#19153 = ORIENTED_EDGE ( 'NONE', *, *, #11675, .F. ) ;
#19154 = FACE_BOUND ( 'NONE', #395, .T. ) ;
#19155 = PLANE ( 'NONE',  #7817 ) ;
#19156 = CARTESIAN_POINT ( 'NONE',  ( -7.499999999999994671, -38.00000000000000000, 1.500000000000000000 ) ) ;
#19157 = LINE ( 'NONE', #11489, #13457 ) ;
#19158 = PLANE ( 'NONE',  #4990 ) ;
#19159 = CARTESIAN_POINT ( 'NONE',  ( -19.24771351637086880, -26.64274437364857206, 35.98632249208304046 ) ) ;
#19160 = CARTESIAN_POINT ( 'NONE',  ( 1.035533905932739751, 61.50000000000000000, 46.24999999999998579 ) ) ;
#19161 = CARTESIAN_POINT ( 'NONE',  ( 1.461580736456473684, 65.46158073645646880, 47.85000000109246798 ) ) ;
#19162 = CARTESIAN_POINT ( 'NONE',  ( -25.00000000000000711, 53.00000000000000711, -25.50000000000000000 ) ) ;
#19163 = CARTESIAN_POINT ( 'NONE',  ( -1.767766952966370209, 65.76776695296638309, 46.69999999999999574 ) ) ;
#19164 = LINE ( 'NONE', #16318, #14914 ) ;
#19165 = AXIS2_PLACEMENT_3D ( 'NONE', #5449, #2595, #13267 ) ;
#19166 = ORIENTED_EDGE ( 'NONE', *, *, #19183, .F. ) ;
#19167 = CARTESIAN_POINT ( 'NONE',  ( -18.78091578003889950, -27.53959229564985378, 7.544927507916956877 ) ) ;
#19168 = CARTESIAN_POINT ( 'NONE',  ( -18.78091578003889950, -27.53959229564985378, 2.294927507916958209 ) ) ;
#19169 = DIRECTION ( 'NONE',  ( -1.000000000000000000, -2.602085213965211135E-16, 0.000000000000000000 ) ) ;
#19170 = CARTESIAN_POINT ( 'NONE',  ( -16.50457296725825174, -19.04416526290807354, 11.26757249208304046 ) ) ;
#19171 = CARTESIAN_POINT ( 'NONE',  ( 2.066987300000001415, 64.00000000000000000, 49.35000000109246798 ) ) ;
#19172 = CARTESIAN_POINT ( 'NONE',  ( -19.99999999999999645, -23.83517299489738051, 2.951177507916958209 ) ) ;
#19173 = CARTESIAN_POINT ( 'NONE',  ( -17.64274437364855430, -28.24771351637087236, 7.326177507916957765 ) ) ;
#19174 = CARTESIAN_POINT ( 'NONE',  ( -4.744034285469996171, -45.28611686177728046, 3.000000000000000000 ) ) ;
#19175 = CARTESIAN_POINT ( 'NONE',  ( -1.461580736456473906, 65.46158073645646880, 49.65000000109246514 ) ) ;
#19176 = CARTESIAN_POINT ( 'NONE',  ( 41.99999999999998579, 3.000000000000002665, -52.00000000000000000 ) ) ;
#19177 = EDGE_CURVE ( 'NONE', #4215, #18430, #8431, .T. ) ;
#19178 = EDGE_CURVE ( 'NONE', #2911, #1370, #15984, .T. ) ;
#19179 = CARTESIAN_POINT ( 'NONE',  ( -41.00000000000000711, 53.00000000000000711, 20.00000000000000000 ) ) ;
#19180 = CLOSED_SHELL ( 'NONE', ( #4870, #16113, #14355, #11286, #9971, #16803, #453, #17094, #17017, #1342, #17344, #15749, #10194, #13862, #8307, #18876, #11612, #10847, #12817, #6571, #7253, #3178, #16457, #3648, #1196, #13608, #15530, #3039, #19240, #7777, #14585, #7931, #13477, #617, #16220, #19110, #12276, #3777, #6721, #15572, #3735, #1006, #4236, #18508, #8939, #15378, #13304, #14866, #3254, #16422, #8061, #15041, #2106, #6738, #18245, #4786, #897, #3399, #6248, #15767, #10896, #14665, #3023, #14722, #11643, #16204, #7197, #10784, #5120, #12855, #16031, #5766, #12153, #8637, #18033, #8085, #1616, #5056, #6667, #17198, #17284, #8184, #9525, #4133, #16612, #2844 ) ) ;
#19181 = CARTESIAN_POINT ( 'NONE',  ( 2.066987300000001415, 64.85617417291294373, 47.80000000109247082 ) ) ;
#19182 = LINE ( 'NONE', #14963, #3174 ) ;
#19183 = EDGE_CURVE ( 'NONE', #15003, #11147, #1480, .T. ) ;
#19184 = CARTESIAN_POINT ( 'NONE',  ( 1.035533905932739751, 61.50000000000000000, 44.75000000218494733 ) ) ;
#19185 = ORIENTED_EDGE ( 'NONE', *, *, #11905, .T. ) ;
#19186 = EDGE_LOOP ( 'NONE', ( #4523, #8800, #1764, #9470 ) ) ;
#19187 = CARTESIAN_POINT ( 'NONE',  ( -20.24501739517669563, -18.99630608921239627, 10.83007249208304046 ) ) ;
#19188 = EDGE_CURVE ( 'NONE', #4896, #5010, #7054, .T. ) ;
#19189 = CARTESIAN_POINT ( 'NONE',  ( -12.35725562635140307, -28.24771351637085459, 3.173822492083041347 ) ) ;
#19191 = ORIENTED_EDGE ( 'NONE', *, *, #12109, .F. ) ;
#19190 = ORIENTED_EDGE ( 'NONE', *, *, #16240, .T. ) ;
#19192 = CARTESIAN_POINT ( 'NONE',  ( -12.92450931948788906, -26.31681416490114245, 0.9824275079169599856 ) ) ;
#19193 = CARTESIAN_POINT ( 'NONE',  ( -8.044165262908093084, -21.95952864787946979, 7.330072492083040459 ) ) ;
#19194 = CYLINDRICAL_SURFACE ( 'NONE', #6018, 1.500000000000001332 ) ;
#19195 = CARTESIAN_POINT ( 'NONE',  ( 0.8561741729129460632, 66.06698729999999387, 48.50000000109246656 ) ) ;
#19196 = VERTEX_POINT ( 'NONE', #8344 ) ;
#19197 = VERTEX_POINT ( 'NONE', #11550 ) ;
#19198 = ADVANCED_FACE ( 'NONE', ( #14316 ), #884, .T. ) ;
#19199 = CARTESIAN_POINT ( 'NONE',  ( 14.99999999999998579, 3.000000000000000000, 23.99999999999997158 ) ) ;
#19200 = EDGE_LOOP ( 'NONE', ( #13714, #1349 ) ) ;
#19201 = EDGE_LOOP ( 'NONE', ( #14042, #15508, #17790, #13886 ) ) ;
#19202 = DIRECTION ( 'NONE',  ( -1.000000000000000000, 0.000000000000000000, 0.000000000000000000 ) ) ;
#19203 = CARTESIAN_POINT ( 'NONE',  ( -32.50000000000000000, 52.00000000000000711, -35.00000000000000000 ) ) ;
#19204 = LINE ( 'NONE', #15091, #17214 ) ;
#19205 = CARTESIAN_POINT ( 'NONE',  ( -1.461580736456473462, 62.53841926354353120, 47.45000000109246230 ) ) ;
#19206 = EDGE_CURVE ( 'NONE', #2670, #4041, #16265, .T. ) ;
#19207 = CYLINDRICAL_SURFACE ( 'NONE', #3472, 4.250000000000000000 ) ;
#19208 = LINE ( 'NONE', #3918, #4576 ) ;
#19209 = DIRECTION ( 'NONE',  ( 0.000000000000000000, 1.000000000000000000, 0.000000000000000000 ) ) ;
#19210 = ORIENTED_EDGE ( 'NONE', *, *, #6546, .T. ) ;
#19212 = ORIENTED_EDGE ( 'NONE', *, *, #18397, .T. ) ;
#19211 = ORIENTED_EDGE ( 'NONE', *, *, #3967, .T. ) ;
#19213 = CARTESIAN_POINT ( 'NONE',  ( -20.00369391078762860, -18.75498260482333279, 3.607427507916956433 ) ) ;
#19214 = LINE ( 'NONE', #4316, #7091 ) ;
#19215 = VERTEX_POINT ( 'NONE', #17944 ) ;
#19216 = ORIENTED_EDGE ( 'NONE', *, *, #18042, .T. ) ;
#19217 = CARTESIAN_POINT ( 'NONE',  ( -17.68048971390462754, -22.64274437364856496, 5.361322492083044011 ) ) ;
#19218 = EDGE_CURVE ( 'NONE', #1372, #18051, #14941, .T. ) ;
#19219 = ADVANCED_FACE ( 'NONE', ( #2936 ), #1571, .T. ) ;
#19220 = LINE ( 'NONE', #6086, #17507 ) ;
#19221 = VERTEX_POINT ( 'NONE', #5692 ) ;
#19222 = ADVANCED_FACE ( 'NONE', ( #17641 ), #10379, .T. ) ;
#19223 = CARTESIAN_POINT ( 'NONE',  ( -17.07549068051210739, -21.68318583509881847, 3.607427507916959097 ) ) ;
#19224 = LINE ( 'NONE', #16477, #16945 ) ;
#19225 = ORIENTED_EDGE ( 'NONE', *, *, #13088, .T. ) ;
#19226 = DIRECTION ( 'NONE',  ( -0.000000000000000000, -0.000000000000000000, -1.000000000000000000 ) ) ;
#19227 = ORIENTED_EDGE ( 'NONE', *, *, #13190, .T. ) ;
#19228 = DIRECTION ( 'NONE',  ( -1.000000000000000000, -0.000000000000000000, -0.000000000000000000 ) ) ;
#19229 = EDGE_CURVE ( 'NONE', #9140, #3001, #19214, .T. ) ;
#19230 = DIRECTION ( 'NONE',  ( -0.000000000000000000, 0.7071067811865452413, 0.7071067811865497932 ) ) ;
#19231 = DIRECTION ( 'NONE',  ( 0.000000000000000000, 0.000000000000000000, -1.000000000000000000 ) ) ;
#19232 = APPLICATION_PROTOCOL_DEFINITION ( 'draft international standard', 'automotive_design', 1998, #14083 ) ;
#19233 = DIRECTION ( 'NONE',  ( 0.000000000000000000, 0.000000000000000000, -1.000000000000000000 ) ) ;
#19234 = CARTESIAN_POINT ( 'NONE',  ( -18.53959229564986799, -20.21908421996107563, 24.60742750791695954 ) ) ;
#19235 = CIRCLE ( 'NONE', #14228, 2.500000000000001776 ) ;
#19236 = CARTESIAN_POINT ( 'NONE',  ( -32.50000000000002132, -0.000000000000000000, -42.50000000000001421 ) ) ;
#19237 = CARTESIAN_POINT ( 'NONE',  ( -17.35725562635144215, -19.58745947852648683, 3.826177507916958209 ) ) ;
#19238 = CARTESIAN_POINT ( 'NONE',  ( -41.00000000000000000, 0.000000000000000000, -50.00000000000000000 ) ) ;
#19239 = VERTEX_POINT ( 'NONE', #10571 ) ;
#19240 = ADVANCED_FACE ( 'NONE', ( #13120 ), #13521, .T. ) ;
#19241 = CARTESIAN_POINT ( 'NONE',  ( -9.999999999999994671, -23.83517299489734143, 2.298822492083040903 ) ) ;
#19242 = EDGE_CURVE ( 'NONE', #717, #2416, #10859, .T. ) ;
#19243 = CARTESIAN_POINT ( 'NONE',  ( -20.24501739517664234, -29.00369391078761439, 7.544927507916956877 ) ) ;
#19244 = CARTESIAN_POINT ( 'NONE',  ( -1.461580736456473906, 65.46158073645646880, 44.65000000109246514 ) ) ;
#19245 = CARTESIAN_POINT ( 'NONE',  ( -17.31681416490117087, -21.92450931948788551, 5.580072492083043123 ) ) ;
#19246 =( GEOMETRIC_REPRESENTATION_CONTEXT ( 3 ) GLOBAL_UNCERTAINTY_ASSIGNED_CONTEXT ( ( #7673 ) ) GLOBAL_UNIT_ASSIGNED_CONTEXT ( ( #15837, #12885, #14458 ) ) REPRESENTATION_CONTEXT ( 'NONE', 'WORKASPACE' ) );
#19247 = CARTESIAN_POINT ( 'NONE',  ( -35.00000000000002132, -6.000000000000000000, -47.50000000000002132 ) ) ;
#19248 = VERTEX_POINT ( 'NONE', #4217 ) ;
#19249 = VECTOR ( 'NONE', #2479, 1000.000000000000000 ) ;
#19250 = CARTESIAN_POINT ( 'NONE',  ( -10.26208722734517842, -21.10617379198820487, 6.318196777486344053E-14 ) ) ;
#19251 = ORIENTED_EDGE ( 'NONE', *, *, #14804, .F. ) ;
#19252 = CARTESIAN_POINT ( 'NONE',  ( 4.130991513055743525, 32.62172003681456545, 53.86292658466342687 ) ) ;
#19253 = CARTESIAN_POINT ( 'NONE',  ( 11.00000000000000355, 0.000000000000000000, 0.000000000000000000 ) ) ;
#19254 = CARTESIAN_POINT ( 'NONE',  ( 4.592425496802577917E-16, 61.50000000000000000, 45.39999999999999858 ) ) ;
#19255 = FACE_OUTER_BOUND ( 'NONE', #8540, .T. ) ;
#19256 = CARTESIAN_POINT ( 'NONE',  ( -17.64274437364858983, -19.75228648362910633, 42.54882249208304046 ) ) ;
#19257 = CARTESIAN_POINT ( 'NONE',  ( 1.767766952966370653, 62.23223304703363112, 47.09999999999999432 ) ) ;
#19258 = CARTESIAN_POINT ( 'NONE',  ( 2.066987300000001415, 64.85617417291294373, 47.00000000109246656 ) ) ;
#19259 = DIRECTION ( 'NONE',  ( -1.541976423090495633E-16, 0.000000000000000000, 1.000000000000000000 ) ) ;
#19260 = CARTESIAN_POINT ( 'NONE',  ( -1.530808498934192803E-16, 66.50000000000000000, 47.39999999999999858 ) ) ;
#19261 = CARTESIAN_POINT ( 'NONE',  ( -8.528048594804062077, -45.28611686177728046, 3.000000000000000000 ) ) ;
#19262 = AXIS2_PLACEMENT_3D ( 'NONE', #4268, #15144, #12192 ) ;
#19263 = EDGE_CURVE ( 'NONE', #18664, #17089, #8911, .T. ) ;
#19264 = ORIENTED_EDGE ( 'NONE', *, *, #12226, .F. ) ;
#19265 = SURFACE_STYLE_FILL_AREA ( #2591 ) ;
#19266 = CARTESIAN_POINT ( 'NONE',  ( -18.53959229564986799, -20.21908421996107563, 3.607427507916956877 ) ) ;
#19267 = CARTESIAN_POINT ( 'NONE',  ( -19.41254052147348830, -26.35725562635142083, 13.01367750791695777 ) ) ;
#19268 = CARTESIAN_POINT ( 'NONE',  ( -2.156160770143801475, 64.48039283663632659, 45.00000000000000000 ) ) ;
#19269 = CARTESIAN_POINT ( 'NONE',  ( -21.14459132904239169, -20.64274437364858628, 42.11132249208304046 ) ) ;
#19270 = CARTESIAN_POINT ( 'NONE',  ( 2.066987300000002303, 63.14382582708705627, 46.10000000109246798 ) ) ;
#19271 = CARTESIAN_POINT ( 'NONE',  ( -14.83517299489738761, -20.99999999999997513, 41.01367750791695954 ) ) ;
#19272 = AXIS2_PLACEMENT_3D ( 'NONE', #13636, #3451, #15507 ) ;
#19273 = DIRECTION ( 'NONE',  ( 0.000000000000000000, 0.000000000000000000, -1.000000000000000000 ) ) ;
#19274 = CARTESIAN_POINT ( 'NONE',  ( 2.500000000000000000, -2.357898499370432610, 3.252606517456513302E-15 ) ) ;
#19275 = AXIS2_PLACEMENT_3D ( 'NONE', #7424, #14877, #12023 ) ;
#19276 = DIRECTION ( 'NONE',  ( 1.000000000000000000, 0.000000000000000000, 2.973811673103096679E-16 ) ) ;
#19277 = CARTESIAN_POINT ( 'NONE',  ( 2.749999999999979128, 118.0000000000000000, 37.49999999999997158 ) ) ;
#19278 = CARTESIAN_POINT ( 'NONE',  ( 2.499999999999992895, 65.03553390593273775, 49.64999999999998437 ) ) ;
#19279 = CARTESIAN_POINT ( 'NONE',  ( -3.065533689247737392, -45.28611686177728046, 1.500000000000000000 ) ) ;
#19280 = DIRECTION ( 'NONE',  ( 1.000000000000000000, 2.312964634635742957E-16, 0.000000000000000000 ) ) ;
#19281 = LINE ( 'NONE', #17706, #1117 ) ;
#19282 = ORIENTED_EDGE ( 'NONE', *, *, #5521, .T. ) ;
#19283 = VERTEX_POINT ( 'NONE', #2324 ) ;
#19284 = CARTESIAN_POINT ( 'NONE',  ( -15.16482700510264436, -16.99999999999997868, 16.73632249208304046 ) ) ;
#19285 = AXIS2_PLACEMENT_3D ( 'NONE', #3612, #9581, #2238 ) ;
#19286 = VECTOR ( 'NONE', #8183, 1000.000000000000000 ) ;
#19287 = LINE ( 'NONE', #14971, #17864 ) ;
#19289 = EDGE_LOOP ( 'NONE', ( #10381, #4093 ) ) ;
#19288 = ORIENTED_EDGE ( 'NONE', *, *, #9244, .T. ) ;
#19290 = PRODUCT_DEFINITION_SHAPE ( 'NONE', 'NONE',  #19146 ) ;
#19291 = CARTESIAN_POINT ( 'NONE',  ( -12.92450931948788906, -26.31681416490114245, 16.73242750791696309 ) ) ;
#19292 = CARTESIAN_POINT ( 'NONE',  ( 1.035533905932739751, 61.50000000000000000, 48.75000000218494023 ) ) ;
#19293 = CARTESIAN_POINT ( 'NONE',  ( -15.16482700510264436, -16.99999999999997868, 11.48632249208304046 ) ) ;
#19294 =( BOUNDED_CURVE ( )  B_SPLINE_CURVE ( 2, ( #8337, #701, #7116, #3827, #14567, #17167, #4185, #14025, #11257, #10243, #14662, #5299, #5126, #9702, #15787, #8250, #1234, #14219, #2802, #10138, #3728, #12559, #17076, #4283, #13081, #17704, #786, #13188, #6773, #16230, #12738, #597, #17260, #8154, #15695, #7216, #9794, #14127, #16137, #19181, #19081, #1139, #18558, #11079, #18734, #9610, #5749, #12648, #2353, #5652, #3639, #15596, #11616, #11711, #2165, #17608, #2705, #6590, #18647, #2264, #5214, #11168, #3094, #14864, #1642, #18007, #9078, #11918, #18104, #8777, #6049, #4787, #3203, #69, #13486, #1731, #10437, #7614, #4483, #5947, #7510, #1437, #10634, #10736, #12007, #13578, #4580, #17807, #2996, #8975, #161, #10538, #6147, #17913, #14770, #16732, #16529 ),
 .UNSPECIFIED., .F., .F. ) 
 B_SPLINE_CURVE_WITH_KNOTS ( ( 3, 2, 2, 2, 2, 2, 2, 2, 2, 2, 2, 2, 2, 2, 2, 2, 2, 2, 2, 2, 2, 2, 2, 2, 2, 2, 2, 2, 2, 2, 2, 2, 2, 2, 2, 2, 2, 2, 2, 2, 2, 2, 2, 2, 2, 2, 2, 2, 3 ),
 ( 0.000000000000000000, 0.01785714285714285615, 0.03571428571428571230, 0.05357142857142856845, 0.07142857142857142461, 0.08928571428571430157, 0.1071428571428571369, 0.1250000000000000000, 0.1428571428571428492, 0.1607142857142857262, 0.1785714285714286031, 0.1964285714285713969, 0.2142857142857142738, 0.2321428571428571508, 0.2500000000000000000, 0.2678571428571428492, 0.2857142857142856984, 0.3035714285714285476, 0.3214285714285714524, 0.3392857142857143016, 0.3571428571428572063, 0.3750000000000000000, 0.3928571428571427937, 0.4107142857142856984, 0.4285714285714285476, 0.4464285714285714524, 0.4642857142857143016, 0.4821428571428572063, 0.5000000000000000000, 0.5178571428571429047, 0.5357142857142856984, 0.5535714285714286031, 0.5714285714285713969, 0.5892857142857143016, 0.6071428571428570953, 0.6250000000000001110, 0.6428571428571429047, 0.6607142857142856984, 0.6785714285714286031, 0.6964285714285713969, 0.7142857142857144126, 0.7321428571428570953, 0.7500000000000000000, 0.7678571428571429047, 0.7857142857142855874, 0.8035714285714286031, 0.8214285714285713969, 0.8392857142857143016, 0.8482142859019456971 ),
 .UNSPECIFIED. ) 
 CURVE ( )  GEOMETRIC_REPRESENTATION_ITEM ( )  RATIONAL_B_SPLINE_CURVE ( ( 1.000000000000000000, 0.9238795325112867385, 1.000000000000000000, 0.9238795325112867385, 1.000000000000000000, 0.9238795325112867385, 1.000000000000000000, 0.9238795325112867385, 1.000000000000000000, 0.9238795325112867385, 1.000000000000000000, 0.9238795325112867385, 1.000000000000000000, 0.9238795325112867385, 1.000000000000000000, 0.9238795325112867385, 1.000000000000000000, 0.9238795325112867385, 1.000000000000000000, 0.9238795325112867385, 1.000000000000000000, 0.9238795325112867385, 1.000000000000000000, 0.9238795325112867385, 1.000000000000000000, 0.9238795325112867385, 1.000000000000000000, 0.9238795325112867385, 1.000000000000000000, 0.9238795325112867385, 1.000000000000000000, 0.9238795325112867385, 1.000000000000000000, 0.9238795325112867385, 1.000000000000000000, 0.9238795325112867385, 1.000000000000000000, 0.9238795325112867385, 1.000000000000000000, 0.9238795325112867385, 1.000000000000000000, 0.9238795325112867385, 1.000000000000000000, 0.9238795325112867385, 1.000000000000000000, 0.9238795325112867385, 1.000000000000000000, 0.9238795325112867385, 1.000000000000000000, 0.9238795325112867385, 1.000000000000000000, 0.9238795325112867385, 1.000000000000000000, 0.9238795325112867385, 1.000000000000000000, 0.9238795325112867385, 1.000000000000000000, 0.9238795325112867385, 1.000000000000000000, 0.9238795325112867385, 1.000000000000000000, 0.9238795325112867385, 1.000000000000000000, 0.9238795325112867385, 1.000000000000000000, 0.9238795325112867385, 1.000000000000000000, 0.9238795325112867385, 1.000000000000000000, 0.9238795325112867385, 1.000000000000000000, 0.9238795325112867385, 1.000000000000000000, 0.9238795325112867385, 1.000000000000000000, 0.9238795325112867385, 1.000000000000000000, 0.9238795325112867385, 1.000000000000000000, 0.9238795325112867385, 1.000000000000000000, 0.9238795325112867385, 1.000000000000000000, 0.9238795325112867385, 1.000000000000000000, 0.9238795325112867385, 1.000000000000000000, 0.9238795325112867385, 1.000000000000000000, 0.9238795325112867385, 1.000000000000000000, 0.9238795325112867385, 1.000000000000000000, 0.9238795325112867385, 1.000000000000000000, 0.9619397654556964827, 0.9619397662556434803 ) ) 
 REPRESENTATION_ITEM ( '' )  );
#19295 = CARTESIAN_POINT ( 'NONE',  ( -8.528048594804062077, -42.28611686177728046, 3.000000000000000000 ) ) ;
#19296 = CARTESIAN_POINT ( 'NONE',  ( -2.066987300000001859, 64.85617417291294373, 49.50000000109246656 ) ) ;
#19297 = VERTEX_POINT ( 'NONE', #14900 ) ;
#19298 = ORIENTED_EDGE ( 'NONE', *, *, #7350, .F. ) ;
#19299 = CARTESIAN_POINT ( 'NONE',  ( 4.592425496802577917E-16, 61.50000000000000000, 46.99999999999999289 ) ) ;
#19300 = CARTESIAN_POINT ( 'NONE',  ( -14.99999999999999645, 3.000000000000000000, 23.99999999999997868 ) ) ;
#19301 = ORIENTED_EDGE ( 'NONE', *, *, #12009, .F. ) ;
#19302 = DIRECTION ( 'NONE',  ( 6.123233995736588542E-17, -1.000000000000000000, 0.000000000000000000 ) ) ;
#19303 = CARTESIAN_POINT ( 'NONE',  ( -2.492551403682614186, 27.92836399182264273, 58.20336399182264131 ) ) ;
#19304 = CIRCLE ( 'NONE', #3960, 2.500000000000000444 ) ;
#19305 = CARTESIAN_POINT ( 'NONE',  ( -1.461580736456473906, 65.46158073645646880, 48.05000000109247082 ) ) ;
#19306 = VECTOR ( 'NONE', #903, 1000.000000000000000 ) ;
#19307 = CARTESIAN_POINT ( 'NONE',  ( -14.99999999999999645, 52.00000000000000711, 23.99999999999997868 ) ) ;
#19308 = EDGE_CURVE ( 'NONE', #5915, #1741, #4936, .T. ) ;
#19309 = CARTESIAN_POINT ( 'NONE',  ( 2.500000000000000000, -1.178949249685214307, 2.042000000000002036 ) ) ;
#19310 = VERTEX_POINT ( 'NONE', #12046 ) ;
#19312 = EDGE_LOOP ( 'NONE', ( #5308, #1939, #12341, #8142 ) ) ;
#19311 = ORIENTED_EDGE ( 'NONE', *, *, #5642, .F. ) ;
#19313 = CARTESIAN_POINT ( 'NONE',  ( -13.28918265808472299, -31.04416526290805933, 17.16992750791696309 ) ) ;
#19314 = DIRECTION ( 'NONE',  ( -2.602085213965211135E-16, 1.000000000000000000, -0.000000000000000000 ) ) ;
#19315 = ORIENTED_EDGE ( 'NONE', *, *, #1761, .T. ) ;
#19316 = VERTEX_POINT ( 'NONE', #7444 ) ;
#19317 = CARTESIAN_POINT ( 'NONE',  ( -15.16482700510262482, -20.99999999999997513, 0.9863224920830429010 ) ) ;
#19318 = EDGE_CURVE ( 'NONE', #5104, #17515, #17290, .T. ) ;
#19319 = AXIS2_PLACEMENT_3D ( 'NONE', #18656, #5221, #6961 ) ;
#19320 = CARTESIAN_POINT ( 'NONE',  ( -41.00000000000000711, 110.0000000000000000, -24.49999999999999645 ) ) ;
#19321 = CARTESIAN_POINT ( 'NONE',  ( -41.00000000000000711, 53.00000000000000711, -25.50000000000000000 ) ) ;
#19322 = EDGE_LOOP ( 'NONE', ( #6649, #6366, #4213, #18388 ) ) ;
#19323 = CARTESIAN_POINT ( 'NONE',  ( -15.16482700510260706, -26.99999999999998579, 6.888677507916960430 ) ) ;
#19324 = CARTESIAN_POINT ( 'NONE',  ( -41.00000000000000711, 53.00000000000000711, -19.00000000000000000 ) ) ;
#19325 = ORIENTED_EDGE ( 'NONE', *, *, #14452, .F. ) ;
#19326 = CARTESIAN_POINT ( 'NONE',  ( 14.99999999999998579, 73.00000000000001421, 23.99999999999997158 ) ) ;
#19327 = ORIENTED_EDGE ( 'NONE', *, *, #17670, .F. ) ;
#19328 = DIRECTION ( 'NONE',  ( 1.000000000000000000, -0.000000000000000000, -0.000000000000000000 ) ) ;
#19329 = FACE_OUTER_BOUND ( 'NONE', #3422, .T. ) ;
#19330 = CARTESIAN_POINT ( 'NONE',  ( -41.00000000000000711, 53.00000000000000711, -25.50000000000000000 ) ) ;
#19331 = APPLICATION_PROTOCOL_DEFINITION ( 'draft international standard', 'automotive_design', 1998, #5081 ) ;
#19332 = CARTESIAN_POINT ( 'NONE',  ( -31.74999999999995737, 0.000000000000000000, 0.000000000000000000 ) ) ;
#19333 = EDGE_CURVE ( 'NONE', #10557, #16562, #10213, .T. ) ;
#19334 = DIRECTION ( 'NONE',  ( 1.000000000000000000, 0.000000000000000000, 0.000000000000000000 ) ) ;
#19335 = EDGE_CURVE ( 'NONE', #14997, #19197, #13412, .T. ) ;
#19336 = DIRECTION ( 'NONE',  ( -0.000000000000000000, -0.000000000000000000, -1.000000000000000000 ) ) ;
#19337 = EDGE_CURVE ( 'NONE', #13561, #8432, #8977, .T. ) ;
#19338 = CARTESIAN_POINT ( 'NONE',  ( -10.75228648362910100, -26.64274437364854009, 6.013677507916958653 ) ) ;
#19339 = DIRECTION ( 'NONE',  ( 0.000000000000000000, 9.912705577010328508E-16, 1.000000000000000000 ) ) ;
#19340 = VERTEX_POINT ( 'NONE', #3131 ) ;
#19341 = CARTESIAN_POINT ( 'NONE',  ( -17.64274437364858983, -19.75228648362910633, 5.798822492083041347 ) ) ;
#19342 = CARTESIAN_POINT ( 'NONE',  ( -14.83517299489740715, -16.99999999999997868, 4.263677507916957765 ) ) ;
#19343 = CARTESIAN_POINT ( 'NONE',  ( -2.066987300000001415, 64.00000000000000000, 44.75000000109247367 ) ) ;
#19344 = CARTESIAN_POINT ( 'NONE',  ( -15.16482700510262482, -20.99999999999997513, 6.236322492083043123 ) ) ;
#19345 = DIRECTION ( 'NONE',  ( 1.000000000000000000, -0.000000000000000000, -0.000000000000000000 ) ) ;
#19346 = ORIENTED_EDGE ( 'NONE', *, *, #665, .T. ) ;
#19347 = CARTESIAN_POINT ( 'NONE',  ( 34.99999999999999289, 0.000000000000000000, 47.49999999999997868 ) ) ;
#19348 = ORIENTED_EDGE ( 'NONE', *, *, #8035, .T. ) ;
#19349 = CARTESIAN_POINT ( 'NONE',  ( -18.53959229564986799, -20.21908421996107563, 40.35742750791696665 ) ) ;
#19350 = DIRECTION ( 'NONE',  ( 0.000000000000000000, -0.000000000000000000, -1.000000000000000000 ) ) ;
#19351 = DIRECTION ( 'NONE',  ( 1.000000000000000000, 0.000000000000000000, 2.973811673103096679E-16 ) ) ;
#19352 = DIRECTION ( 'NONE',  ( 0.000000000000000000, -1.000000000000000000, 0.000000000000000000 ) ) ;
#19353 = LINE ( 'NONE', #4848, #7214 ) ;
#19354 = CARTESIAN_POINT ( 'NONE',  ( 2.066987300000001415, 64.85617417291294373, 46.20000000109248361 ) ) ;
#19355 = EDGE_CURVE ( 'NONE', #3881, #4896, #17742, .T. ) ;
#19356 = CARTESIAN_POINT ( 'NONE',  ( -37.50000000000002132, 0.000000000000000000, -25.00000000000002132 ) ) ;
#19357 = CARTESIAN_POINT ( 'NONE',  ( -2.500000000000001776, 64.00000000000000000, 46.79999999999999716 ) ) ;
#19358 = DIRECTION ( 'NONE',  ( 0.000000000000000000, 0.000000000000000000, 1.000000000000000000 ) ) ;
#19359 = ORIENTED_EDGE ( 'NONE', *, *, #4892, .T. ) ;
#19360 = AXIS2_PLACEMENT_3D ( 'NONE', #13576, #157, #18102 ) ;
#19361 = CARTESIAN_POINT ( 'NONE',  ( -17.64274437364855430, -28.24771351637087236, 2.076177507916958209 ) ) ;
#19362 = CARTESIAN_POINT ( 'NONE',  ( -20.04416526290808065, -25.17491895705300209, 18.48242750791695954 ) ) ;
#19363 = CARTESIAN_POINT ( 'NONE',  ( -2.125375761220501758, 64.66924286904182395, 45.00000000000002842 ) ) ;
#19364 = CARTESIAN_POINT ( 'NONE',  ( -14.83517299489734853, -30.99999999999998224, 40.36132249208304046 ) ) ;
#19365 = CARTESIAN_POINT ( 'NONE',  ( 49.99999999999998579, 3.000000000000000000, 59.99999999999997868 ) ) ;
#19366 = CARTESIAN_POINT ( 'NONE',  ( -18.78091578003889950, -27.53959229564985378, 7.544927507916956877 ) ) ;
#19367 = CARTESIAN_POINT ( 'NONE',  ( 43.50000000000001421, 115.0000000000000000, 32.49999999999998579 ) ) ;
#19368 = CARTESIAN_POINT ( 'NONE',  ( -20.04416526290808065, -25.17491895705300209, 7.982427507916958653 ) ) ;
#19369 = CARTESIAN_POINT ( 'NONE',  ( 50.00000000000000000, 3.000000000000000000, -60.00000000000000000 ) ) ;
#19370 = EDGE_CURVE ( 'NONE', #18722, #17318, #17842, .T. ) ;
#19371 = CYLINDRICAL_SURFACE ( 'NONE', #607, 1.500000000000001332 ) ;
#19372 = LINE ( 'NONE', #254, #5588 ) ;
#19373 = VECTOR ( 'NONE', #17699, 1000.000000000000114 ) ;
#19374 = LINE ( 'NONE', #2704, #3182 ) ;
#19375 = FACE_OUTER_BOUND ( 'NONE', #5218, .T. ) ;
#19376 = PLANE ( 'NONE',  #10660 ) ;
#19377 = CARTESIAN_POINT ( 'NONE',  ( 3.999999999999998224, 67.00000000000000000, 34.99999999999999289 ) ) ;
#19378 = ORIENTED_EDGE ( 'NONE', *, *, #4171, .T. ) ;
#19379 = EDGE_CURVE ( 'NONE', #19091, #14106, #6500, .T. ) ;
#19380 = ORIENTED_EDGE ( 'NONE', *, *, #4509, .T. ) ;
#19381 = CARTESIAN_POINT ( 'NONE',  ( -20.24501739517669563, -18.99630608921239627, 16.08007249208304046 ) ) ;
#19382 = VECTOR ( 'NONE', #11808, 1000.000000000000000 ) ;
#19383 = DIRECTION ( 'NONE',  ( 0.000000000000000000, -0.000000000000000000, -1.000000000000000000 ) ) ;
#19385 = ORIENTED_EDGE ( 'NONE', *, *, #5333, .T. ) ;
#19384 = ORIENTED_EDGE ( 'NONE', *, *, #16364, .T. ) ;
#19386 = CARTESIAN_POINT ( 'NONE',  ( -12.04416526290807887, -24.96867458239596260, 21.54492750791695954 ) ) ;
#19387 = DIRECTION ( 'NONE',  ( -1.000000000000000000, 0.000000000000000000, -1.541976423090495633E-16 ) ) ;
#19388 = CARTESIAN_POINT ( 'NONE',  ( -20.97976432393974022, -27.64274437364858628, 9.736322492083036906 ) ) ;
#19389 = CARTESIAN_POINT ( 'NONE',  ( 1.461580736456473906, 62.53841926354353120, 48.25000000109246656 ) ) ;
#19390 = CARTESIAN_POINT ( 'NONE',  ( -2.500000000000000888, 62.96446609406726935, 44.55000000218495870 ) ) ;
#19391 = ORIENTED_EDGE ( 'NONE', *, *, #10310, .F. ) ;
#19392 = ORIENTED_EDGE ( 'NONE', *, *, #13702, .F. ) ;
#19393 = DIRECTION ( 'NONE',  ( 1.000000000000000000, -0.000000000000000000, -0.000000000000000000 ) ) ;
#19394 = VERTEX_POINT ( 'NONE', #2049 ) ;
#19395 = NEXT_ASSEMBLY_USAGE_OCCURRENCE ( 'NAUO1', ' ', ' ', #11688, #15783, $ ) ;
#19396 = NEXT_ASSEMBLY_USAGE_OCCURRENCE ( 'NAUO2', ' ', ' ', #11688, #9182, $ ) ;
#19397 = NEXT_ASSEMBLY_USAGE_OCCURRENCE ( 'NAUO3', ' ', ' ', #11688, #19146, $ ) ;
#19398 = NEXT_ASSEMBLY_USAGE_OCCURRENCE ( 'NAUO4', ' ', ' ', #11688, #6693, $ ) ;
#19399 = NEXT_ASSEMBLY_USAGE_OCCURRENCE ( 'NAUO5', ' ', ' ', #11688, #13627, $ ) ;
#19400 = NEXT_ASSEMBLY_USAGE_OCCURRENCE ( 'NAUO6', ' ', ' ', #11688, #12776, $ ) ;
#19401 = NEXT_ASSEMBLY_USAGE_OCCURRENCE ( 'NAUO7', ' ', ' ', #11688, #16256, $ ) ;
#19402 = NEXT_ASSEMBLY_USAGE_OCCURRENCE ( 'NAUO8', ' ', ' ', #11688, #4165, $ ) ;
#19403 = NEXT_ASSEMBLY_USAGE_OCCURRENCE ( 'NAUO9', ' ', ' ', #11688, #7639, $ ) ;
#19404 = NEXT_ASSEMBLY_USAGE_OCCURRENCE ( 'NAUO10', ' ', ' ', #11688, #9182, $ ) ;
#19405 = NEXT_ASSEMBLY_USAGE_OCCURRENCE ( 'NAUO11', ' ', ' ', #11688, #13627, $ ) ;
#19406 = NEXT_ASSEMBLY_USAGE_OCCURRENCE ( 'NAUO12', ' ', ' ', #11688, #18072, $ ) ;
#19407 = NEXT_ASSEMBLY_USAGE_OCCURRENCE ( 'NAUO13', ' ', ' ', #11688, #18072, $ ) ;
#19408 = NEXT_ASSEMBLY_USAGE_OCCURRENCE ( 'NAUO14', ' ', ' ', #11688, #18072, $ ) ;
#19409 = NEXT_ASSEMBLY_USAGE_OCCURRENCE ( 'NAUO15', ' ', ' ', #11688, #18072, $ ) ;
#19410 = NEXT_ASSEMBLY_USAGE_OCCURRENCE ( 'NAUO16', ' ', ' ', #11688, #12552, $ ) ;
#19411 = NEXT_ASSEMBLY_USAGE_OCCURRENCE ( 'NAUO17', ' ', ' ', #11688, #12552, $ ) ;
#19412 = NEXT_ASSEMBLY_USAGE_OCCURRENCE ( 'NAUO18', ' ', ' ', #11688, #12552, $ ) ;
#19413 = NEXT_ASSEMBLY_USAGE_OCCURRENCE ( 'NAUO19', ' ', ' ', #11688, #12552, $ ) ;
ENDSEC;
END-ISO-10303-21;
